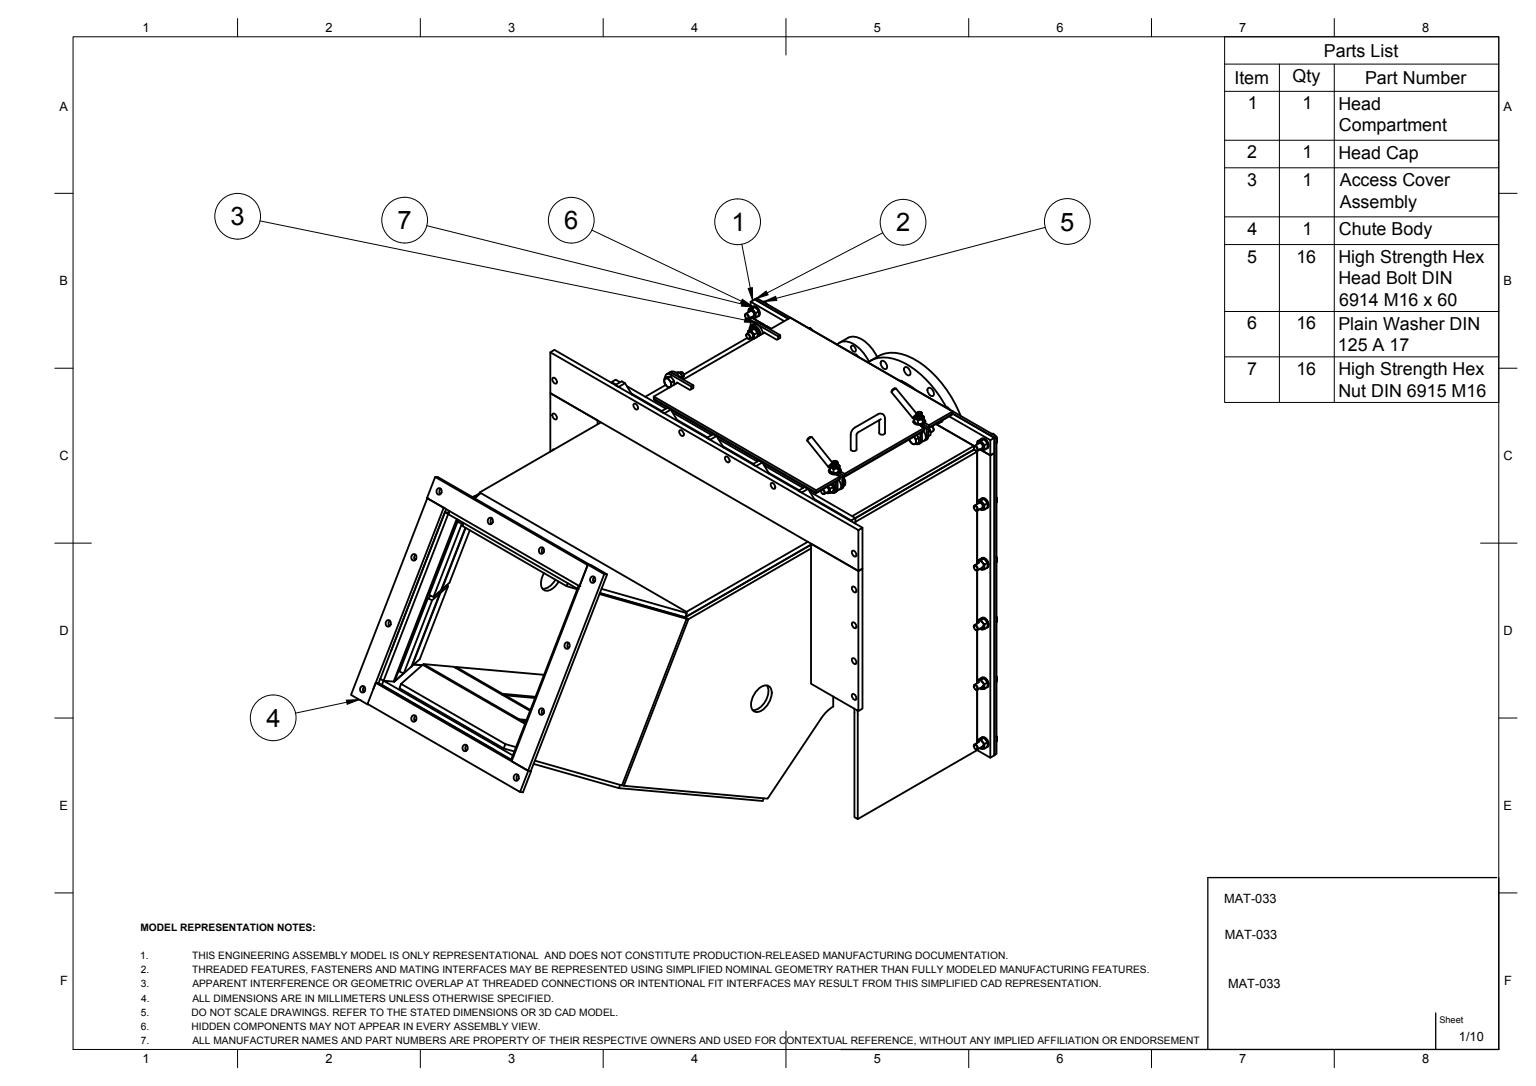
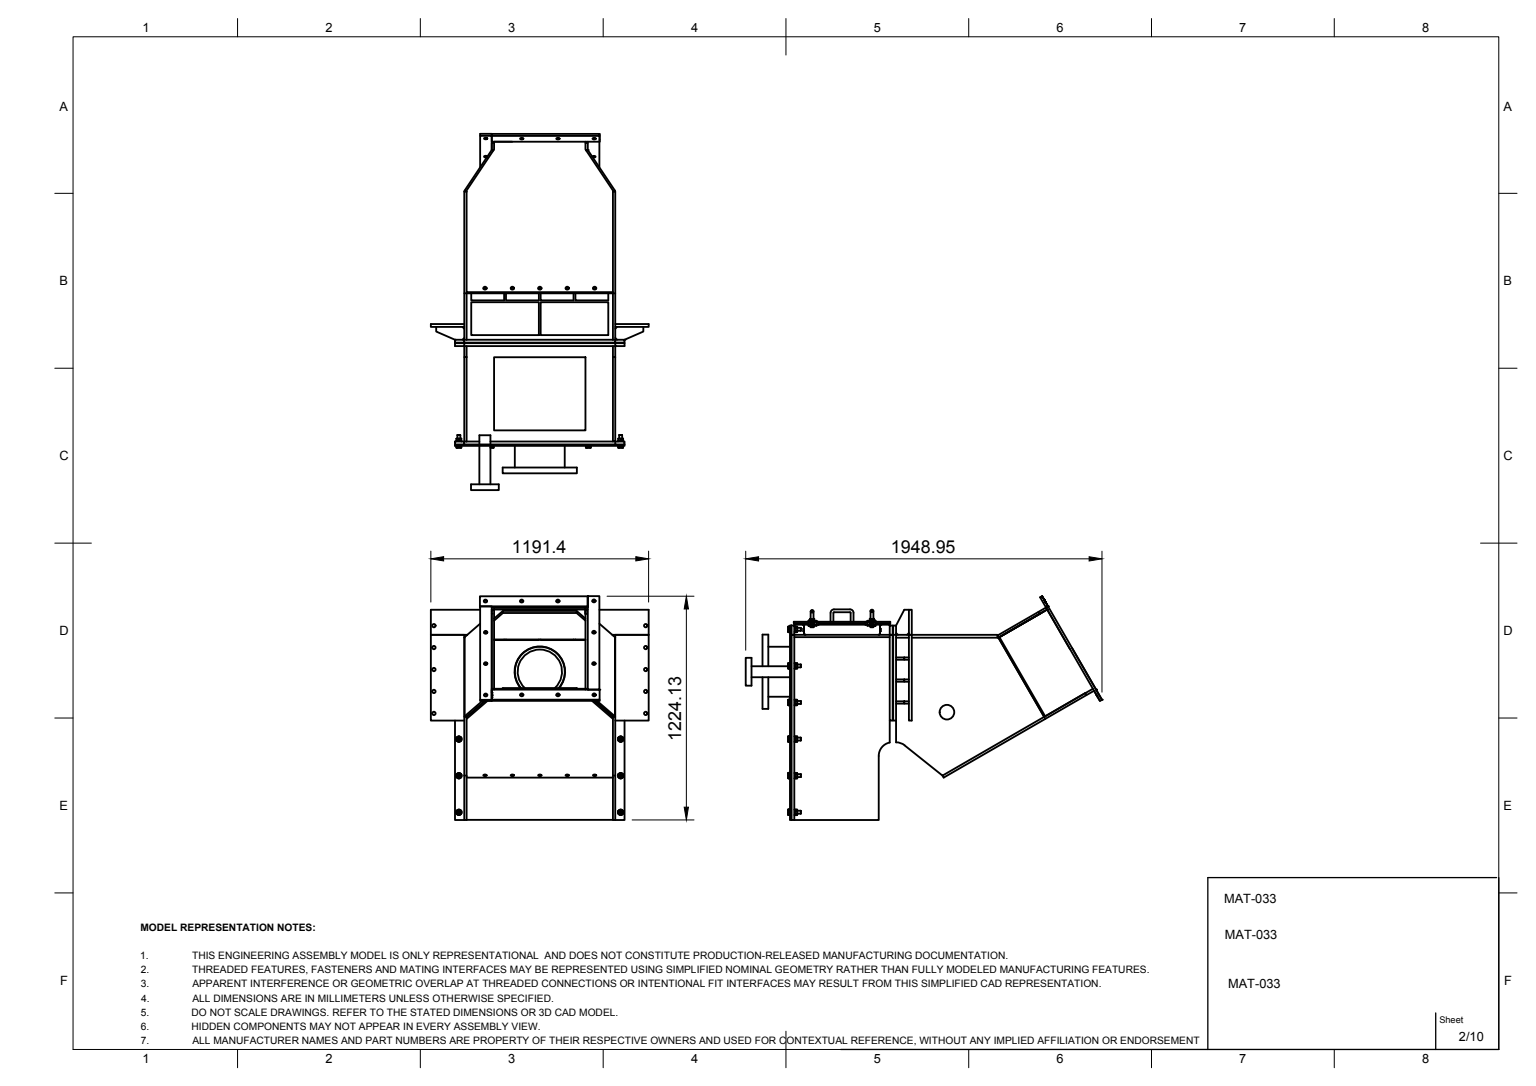
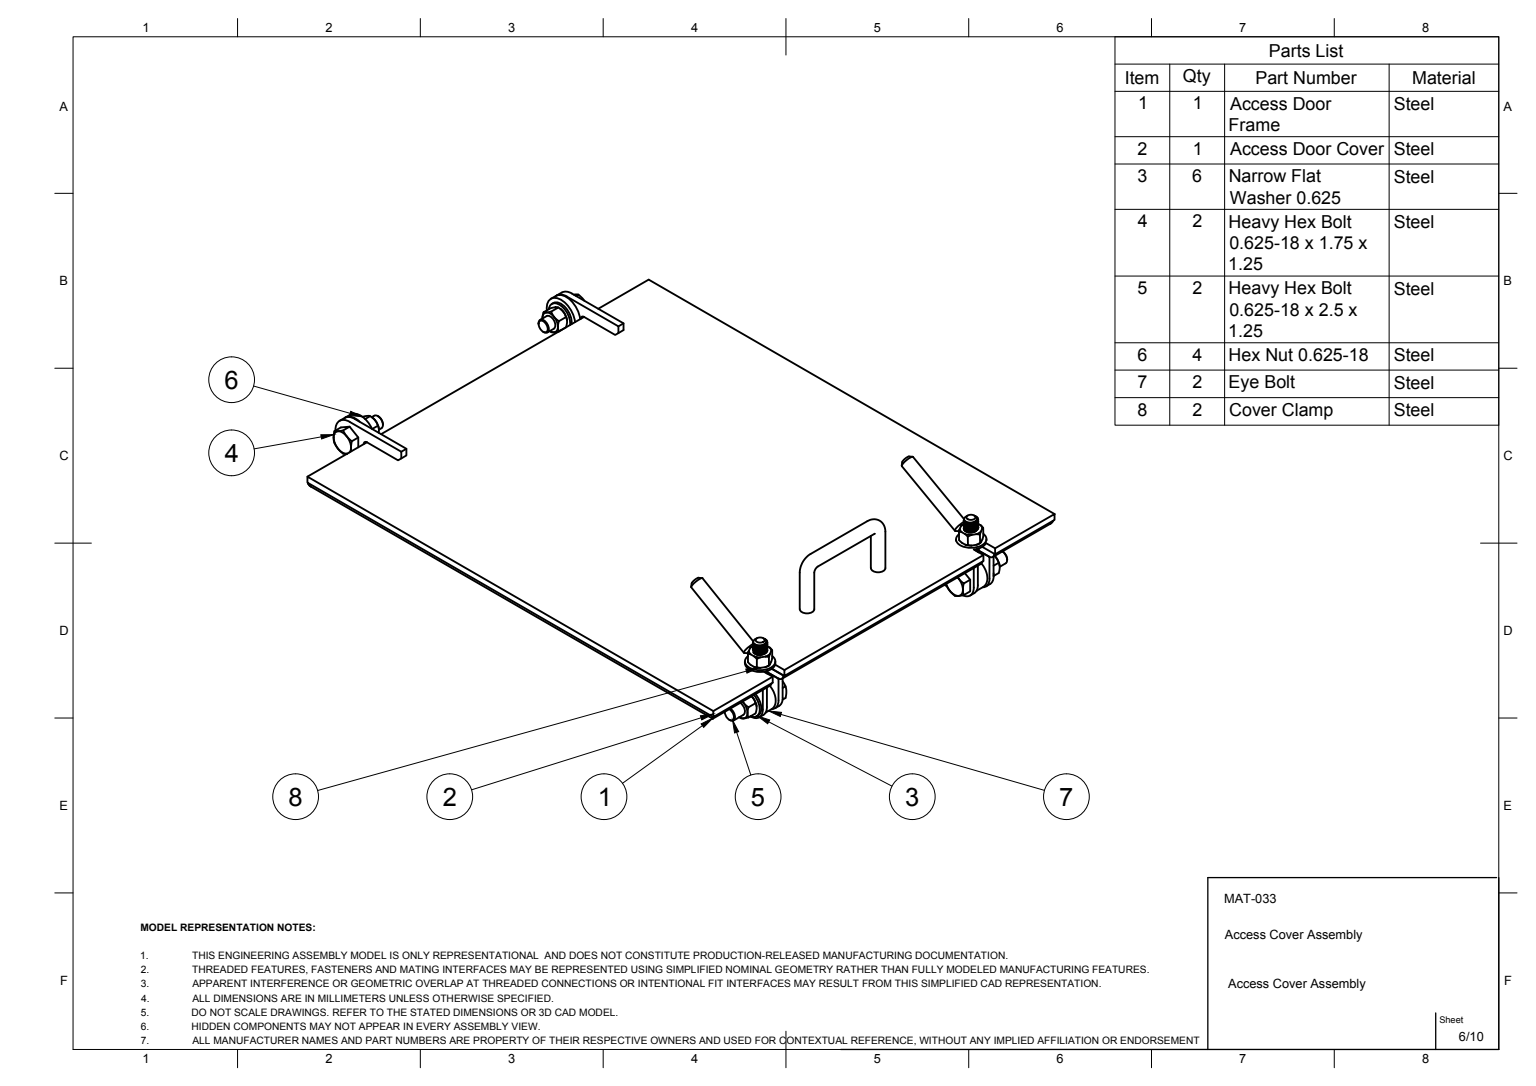
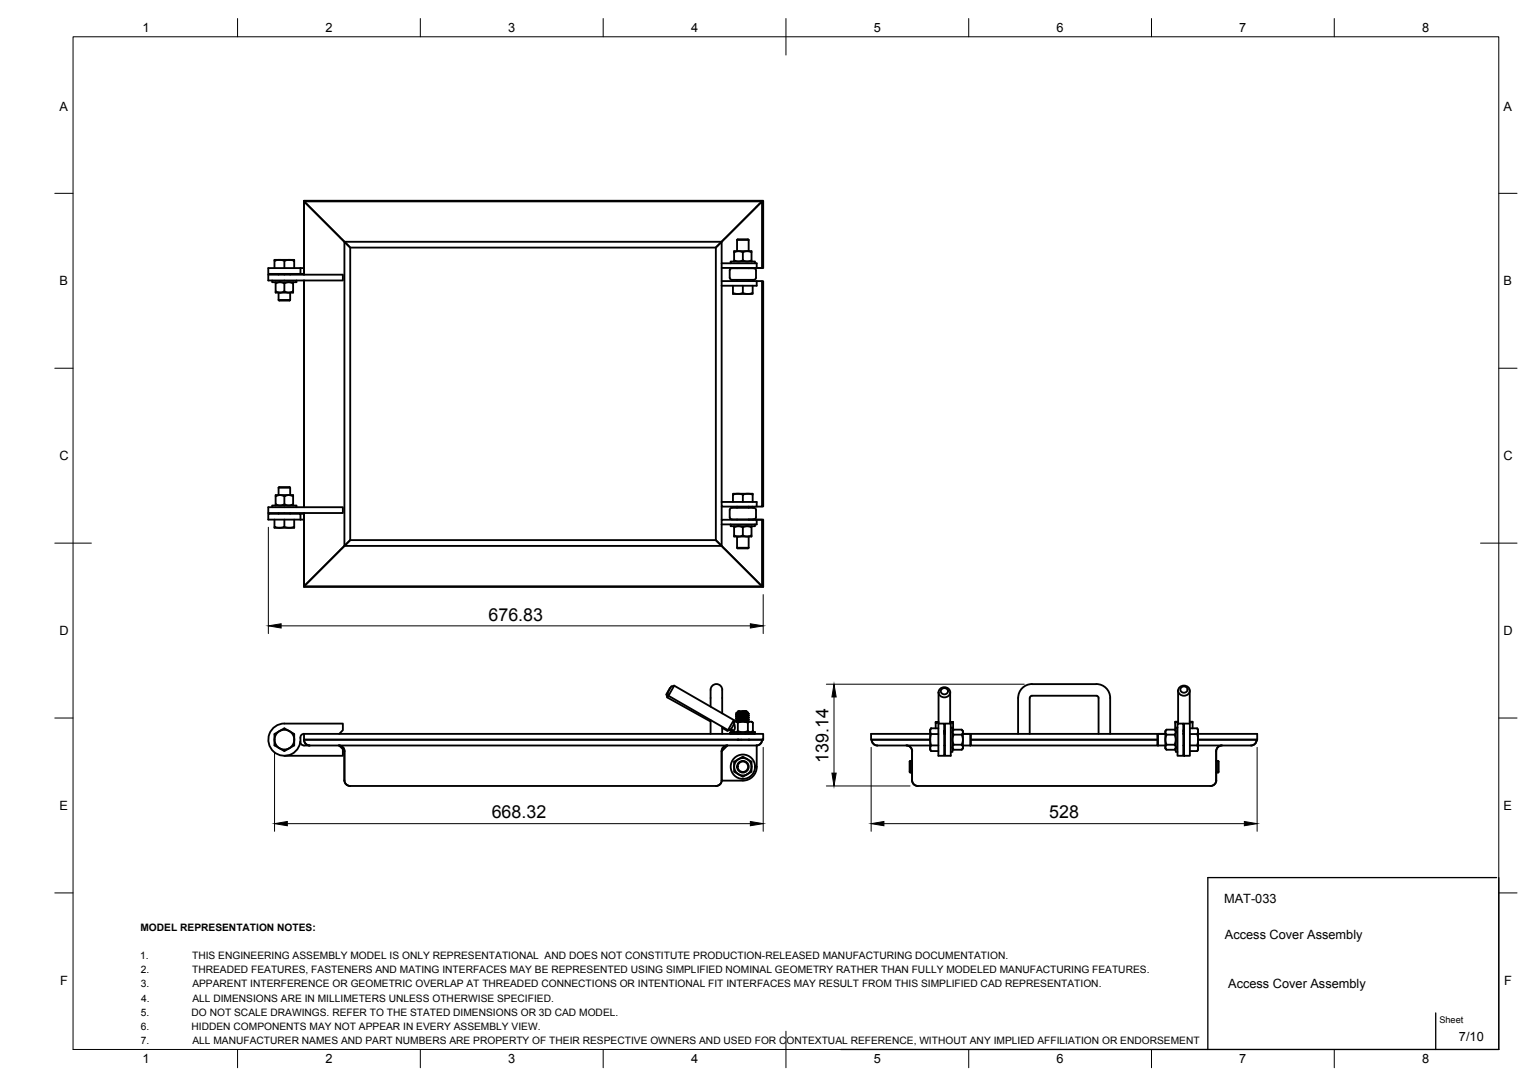
ISO-10303-21;
HEADER;
/* Generated by software containing ST-Developer
 * from STEP Tools, Inc. (www.steptools.com) 
 */

FILE_DESCRIPTION(
/* description */ ('STEP AP214'),
/* implementation_level */ '2;1');

FILE_NAME(
/* name */ 'MAT-033.step',
/* time_stamp */ '2026-11-14T07:13:32-08:00',
/* author */ (''),
/* organization */ (''),
/* preprocessor_version */ 'ST-DEVELOPER v20.2',
/* originating_system */ 'Autodesk Translation Framework v15.17.0.0',
/* authorisation */ '');

FILE_SCHEMA (('AUTOMOTIVE_DESIGN { 1 0 10303 214 3 1 1 }'));
ENDSEC;

DATA;
#10=MECHANICAL_DESIGN_GEOMETRIC_PRESENTATION_REPRESENTATION('',(#1291,#1292,
#1293,#1294,#1295,#1296,#1297,#1298,#1299,#1300,#1301,#1302,#1303,#1304,
#1305,#1306,#1307,#1308,#1309,#1310,#1311,#1312,#1313,#1314,#1315,#1316,
#1317,#1318,#1319,#1320,#1321,#1322,#1323,#1324,#1325,#1326,#1327,#1328,
#1329,#1330,#1331,#1332,#1333,#1334,#1335,#1336,#1337,#1338,#1339,#1340,
#1341,#1342,#1343,#1344,#1345,#1346,#1347,#1348,#1349,#1350,#1351,#1352,
#1353,#1354,#1355,#1356,#1357,#1358,#1359,#1360,#1361,#1362,#1363,#1364,
#1365,#1366,#1367,#1368,#1369,#1370,#1371,#1372,#1373,#1374,#1375,#1376,
#1377,#1378,#1379),#32903);
#11=ITEM_DEFINED_TRANSFORMATION($,$,#16041,#16528);
#12=ITEM_DEFINED_TRANSFORMATION($,$,#16210,#16529);
#13=ITEM_DEFINED_TRANSFORMATION($,$,#16519,#16530);
#14=ITEM_DEFINED_TRANSFORMATION($,$,#16276,#16531);
#15=ITEM_DEFINED_TRANSFORMATION($,$,#16303,#16532);
#16=ITEM_DEFINED_TRANSFORMATION($,$,#16330,#16533);
#17=ITEM_DEFINED_TRANSFORMATION($,$,#16374,#16534);
#18=ITEM_DEFINED_TRANSFORMATION($,$,#16451,#16535);
#19=ITEM_DEFINED_TRANSFORMATION($,$,#16519,#16536);
#20=ITEM_DEFINED_TRANSFORMATION($,$,#16519,#16537);
#21=ITEM_DEFINED_TRANSFORMATION($,$,#16519,#16538);
#22=ITEM_DEFINED_TRANSFORMATION($,$,#16276,#16539);
#23=ITEM_DEFINED_TRANSFORMATION($,$,#16303,#16540);
#24=ITEM_DEFINED_TRANSFORMATION($,$,#16330,#16541);
#25=ITEM_DEFINED_TRANSFORMATION($,$,#16330,#16542);
#26=ITEM_DEFINED_TRANSFORMATION($,$,#16330,#16543);
#27=ITEM_DEFINED_TRANSFORMATION($,$,#16374,#16544);
#28=ITEM_DEFINED_TRANSFORMATION($,$,#16519,#16545);
#29=ITEM_DEFINED_TRANSFORMATION($,$,#16451,#16546);
#30=ITEM_DEFINED_TRANSFORMATION($,$,#16519,#16547);
#31=ITEM_DEFINED_TRANSFORMATION($,$,#15784,#17105);
#32=ITEM_DEFINED_TRANSFORMATION($,$,#15899,#17106);
#33=ITEM_DEFINED_TRANSFORMATION($,$,#16040,#17107);
#34=ITEM_DEFINED_TRANSFORMATION($,$,#16548,#17108);
#35=ITEM_DEFINED_TRANSFORMATION($,$,#17007,#17109);
#36=ITEM_DEFINED_TRANSFORMATION($,$,#17052,#17110);
#37=ITEM_DEFINED_TRANSFORMATION($,$,#17061,#17111);
#38=ITEM_DEFINED_TRANSFORMATION($,$,#17007,#17112);
#39=ITEM_DEFINED_TRANSFORMATION($,$,#17007,#17113);
#40=ITEM_DEFINED_TRANSFORMATION($,$,#17007,#17114);
#41=ITEM_DEFINED_TRANSFORMATION($,$,#17007,#17115);
#42=ITEM_DEFINED_TRANSFORMATION($,$,#17007,#17116);
#43=ITEM_DEFINED_TRANSFORMATION($,$,#17007,#17117);
#44=ITEM_DEFINED_TRANSFORMATION($,$,#17007,#17118);
#45=ITEM_DEFINED_TRANSFORMATION($,$,#17007,#17119);
#46=ITEM_DEFINED_TRANSFORMATION($,$,#17007,#17120);
#47=ITEM_DEFINED_TRANSFORMATION($,$,#17007,#17121);
#48=ITEM_DEFINED_TRANSFORMATION($,$,#17007,#17122);
#49=ITEM_DEFINED_TRANSFORMATION($,$,#17007,#17123);
#50=ITEM_DEFINED_TRANSFORMATION($,$,#17007,#17124);
#51=ITEM_DEFINED_TRANSFORMATION($,$,#17007,#17125);
#52=ITEM_DEFINED_TRANSFORMATION($,$,#17007,#17126);
#53=ITEM_DEFINED_TRANSFORMATION($,$,#17052,#17127);
#54=ITEM_DEFINED_TRANSFORMATION($,$,#17052,#17128);
#55=ITEM_DEFINED_TRANSFORMATION($,$,#17052,#17129);
#56=ITEM_DEFINED_TRANSFORMATION($,$,#17052,#17130);
#57=ITEM_DEFINED_TRANSFORMATION($,$,#17052,#17131);
#58=ITEM_DEFINED_TRANSFORMATION($,$,#17052,#17132);
#59=ITEM_DEFINED_TRANSFORMATION($,$,#17052,#17133);
#60=ITEM_DEFINED_TRANSFORMATION($,$,#17052,#17134);
#61=ITEM_DEFINED_TRANSFORMATION($,$,#17052,#17135);
#62=ITEM_DEFINED_TRANSFORMATION($,$,#17052,#17136);
#63=ITEM_DEFINED_TRANSFORMATION($,$,#17052,#17137);
#64=ITEM_DEFINED_TRANSFORMATION($,$,#17052,#17138);
#65=ITEM_DEFINED_TRANSFORMATION($,$,#17052,#17139);
#66=ITEM_DEFINED_TRANSFORMATION($,$,#17052,#17140);
#67=ITEM_DEFINED_TRANSFORMATION($,$,#17052,#17141);
#68=ITEM_DEFINED_TRANSFORMATION($,$,#17061,#17142);
#69=ITEM_DEFINED_TRANSFORMATION($,$,#17061,#17143);
#70=ITEM_DEFINED_TRANSFORMATION($,$,#17061,#17144);
#71=ITEM_DEFINED_TRANSFORMATION($,$,#17061,#17145);
#72=ITEM_DEFINED_TRANSFORMATION($,$,#17061,#17146);
#73=ITEM_DEFINED_TRANSFORMATION($,$,#17061,#17147);
#74=ITEM_DEFINED_TRANSFORMATION($,$,#17061,#17148);
#75=ITEM_DEFINED_TRANSFORMATION($,$,#17061,#17149);
#76=ITEM_DEFINED_TRANSFORMATION($,$,#17061,#17150);
#77=ITEM_DEFINED_TRANSFORMATION($,$,#17061,#17151);
#78=ITEM_DEFINED_TRANSFORMATION($,$,#17061,#17152);
#79=ITEM_DEFINED_TRANSFORMATION($,$,#17061,#17153);
#80=ITEM_DEFINED_TRANSFORMATION($,$,#17061,#17154);
#81=ITEM_DEFINED_TRANSFORMATION($,$,#17061,#17155);
#82=ITEM_DEFINED_TRANSFORMATION($,$,#17061,#17156);
#83=(
REPRESENTATION_RELATIONSHIP($,$,#33016,#33015)
REPRESENTATION_RELATIONSHIP_WITH_TRANSFORMATION(#11)
SHAPE_REPRESENTATION_RELATIONSHIP()
);
#84=(
REPRESENTATION_RELATIONSHIP($,$,#33017,#33015)
REPRESENTATION_RELATIONSHIP_WITH_TRANSFORMATION(#12)
SHAPE_REPRESENTATION_RELATIONSHIP()
);
#85=(
REPRESENTATION_RELATIONSHIP($,$,#33023,#33015)
REPRESENTATION_RELATIONSHIP_WITH_TRANSFORMATION(#13)
SHAPE_REPRESENTATION_RELATIONSHIP()
);
#86=(
REPRESENTATION_RELATIONSHIP($,$,#33018,#33015)
REPRESENTATION_RELATIONSHIP_WITH_TRANSFORMATION(#14)
SHAPE_REPRESENTATION_RELATIONSHIP()
);
#87=(
REPRESENTATION_RELATIONSHIP($,$,#33019,#33015)
REPRESENTATION_RELATIONSHIP_WITH_TRANSFORMATION(#15)
SHAPE_REPRESENTATION_RELATIONSHIP()
);
#88=(
REPRESENTATION_RELATIONSHIP($,$,#33020,#33015)
REPRESENTATION_RELATIONSHIP_WITH_TRANSFORMATION(#16)
SHAPE_REPRESENTATION_RELATIONSHIP()
);
#89=(
REPRESENTATION_RELATIONSHIP($,$,#33021,#33015)
REPRESENTATION_RELATIONSHIP_WITH_TRANSFORMATION(#17)
SHAPE_REPRESENTATION_RELATIONSHIP()
);
#90=(
REPRESENTATION_RELATIONSHIP($,$,#33022,#33015)
REPRESENTATION_RELATIONSHIP_WITH_TRANSFORMATION(#18)
SHAPE_REPRESENTATION_RELATIONSHIP()
);
#91=(
REPRESENTATION_RELATIONSHIP($,$,#33023,#33015)
REPRESENTATION_RELATIONSHIP_WITH_TRANSFORMATION(#19)
SHAPE_REPRESENTATION_RELATIONSHIP()
);
#92=(
REPRESENTATION_RELATIONSHIP($,$,#33023,#33015)
REPRESENTATION_RELATIONSHIP_WITH_TRANSFORMATION(#20)
SHAPE_REPRESENTATION_RELATIONSHIP()
);
#93=(
REPRESENTATION_RELATIONSHIP($,$,#33023,#33015)
REPRESENTATION_RELATIONSHIP_WITH_TRANSFORMATION(#21)
SHAPE_REPRESENTATION_RELATIONSHIP()
);
#94=(
REPRESENTATION_RELATIONSHIP($,$,#33018,#33015)
REPRESENTATION_RELATIONSHIP_WITH_TRANSFORMATION(#22)
SHAPE_REPRESENTATION_RELATIONSHIP()
);
#95=(
REPRESENTATION_RELATIONSHIP($,$,#33019,#33015)
REPRESENTATION_RELATIONSHIP_WITH_TRANSFORMATION(#23)
SHAPE_REPRESENTATION_RELATIONSHIP()
);
#96=(
REPRESENTATION_RELATIONSHIP($,$,#33020,#33015)
REPRESENTATION_RELATIONSHIP_WITH_TRANSFORMATION(#24)
SHAPE_REPRESENTATION_RELATIONSHIP()
);
#97=(
REPRESENTATION_RELATIONSHIP($,$,#33020,#33015)
REPRESENTATION_RELATIONSHIP_WITH_TRANSFORMATION(#25)
SHAPE_REPRESENTATION_RELATIONSHIP()
);
#98=(
REPRESENTATION_RELATIONSHIP($,$,#33020,#33015)
REPRESENTATION_RELATIONSHIP_WITH_TRANSFORMATION(#26)
SHAPE_REPRESENTATION_RELATIONSHIP()
);
#99=(
REPRESENTATION_RELATIONSHIP($,$,#33021,#33015)
REPRESENTATION_RELATIONSHIP_WITH_TRANSFORMATION(#27)
SHAPE_REPRESENTATION_RELATIONSHIP()
);
#100=(
REPRESENTATION_RELATIONSHIP($,$,#33023,#33015)
REPRESENTATION_RELATIONSHIP_WITH_TRANSFORMATION(#28)
SHAPE_REPRESENTATION_RELATIONSHIP()
);
#101=(
REPRESENTATION_RELATIONSHIP($,$,#33022,#33015)
REPRESENTATION_RELATIONSHIP_WITH_TRANSFORMATION(#29)
SHAPE_REPRESENTATION_RELATIONSHIP()
);
#102=(
REPRESENTATION_RELATIONSHIP($,$,#33023,#33015)
REPRESENTATION_RELATIONSHIP_WITH_TRANSFORMATION(#30)
SHAPE_REPRESENTATION_RELATIONSHIP()
);
#103=(
REPRESENTATION_RELATIONSHIP($,$,#33013,#33012)
REPRESENTATION_RELATIONSHIP_WITH_TRANSFORMATION(#31)
SHAPE_REPRESENTATION_RELATIONSHIP()
);
#104=(
REPRESENTATION_RELATIONSHIP($,$,#33014,#33012)
REPRESENTATION_RELATIONSHIP_WITH_TRANSFORMATION(#32)
SHAPE_REPRESENTATION_RELATIONSHIP()
);
#105=(
REPRESENTATION_RELATIONSHIP($,$,#33015,#33012)
REPRESENTATION_RELATIONSHIP_WITH_TRANSFORMATION(#33)
SHAPE_REPRESENTATION_RELATIONSHIP()
);
#106=(
REPRESENTATION_RELATIONSHIP($,$,#33024,#33012)
REPRESENTATION_RELATIONSHIP_WITH_TRANSFORMATION(#34)
SHAPE_REPRESENTATION_RELATIONSHIP()
);
#107=(
REPRESENTATION_RELATIONSHIP($,$,#33025,#33012)
REPRESENTATION_RELATIONSHIP_WITH_TRANSFORMATION(#35)
SHAPE_REPRESENTATION_RELATIONSHIP()
);
#108=(
REPRESENTATION_RELATIONSHIP($,$,#33026,#33012)
REPRESENTATION_RELATIONSHIP_WITH_TRANSFORMATION(#36)
SHAPE_REPRESENTATION_RELATIONSHIP()
);
#109=(
REPRESENTATION_RELATIONSHIP($,$,#33027,#33012)
REPRESENTATION_RELATIONSHIP_WITH_TRANSFORMATION(#37)
SHAPE_REPRESENTATION_RELATIONSHIP()
);
#110=(
REPRESENTATION_RELATIONSHIP($,$,#33025,#33012)
REPRESENTATION_RELATIONSHIP_WITH_TRANSFORMATION(#38)
SHAPE_REPRESENTATION_RELATIONSHIP()
);
#111=(
REPRESENTATION_RELATIONSHIP($,$,#33025,#33012)
REPRESENTATION_RELATIONSHIP_WITH_TRANSFORMATION(#39)
SHAPE_REPRESENTATION_RELATIONSHIP()
);
#112=(
REPRESENTATION_RELATIONSHIP($,$,#33025,#33012)
REPRESENTATION_RELATIONSHIP_WITH_TRANSFORMATION(#40)
SHAPE_REPRESENTATION_RELATIONSHIP()
);
#113=(
REPRESENTATION_RELATIONSHIP($,$,#33025,#33012)
REPRESENTATION_RELATIONSHIP_WITH_TRANSFORMATION(#41)
SHAPE_REPRESENTATION_RELATIONSHIP()
);
#114=(
REPRESENTATION_RELATIONSHIP($,$,#33025,#33012)
REPRESENTATION_RELATIONSHIP_WITH_TRANSFORMATION(#42)
SHAPE_REPRESENTATION_RELATIONSHIP()
);
#115=(
REPRESENTATION_RELATIONSHIP($,$,#33025,#33012)
REPRESENTATION_RELATIONSHIP_WITH_TRANSFORMATION(#43)
SHAPE_REPRESENTATION_RELATIONSHIP()
);
#116=(
REPRESENTATION_RELATIONSHIP($,$,#33025,#33012)
REPRESENTATION_RELATIONSHIP_WITH_TRANSFORMATION(#44)
SHAPE_REPRESENTATION_RELATIONSHIP()
);
#117=(
REPRESENTATION_RELATIONSHIP($,$,#33025,#33012)
REPRESENTATION_RELATIONSHIP_WITH_TRANSFORMATION(#45)
SHAPE_REPRESENTATION_RELATIONSHIP()
);
#118=(
REPRESENTATION_RELATIONSHIP($,$,#33025,#33012)
REPRESENTATION_RELATIONSHIP_WITH_TRANSFORMATION(#46)
SHAPE_REPRESENTATION_RELATIONSHIP()
);
#119=(
REPRESENTATION_RELATIONSHIP($,$,#33025,#33012)
REPRESENTATION_RELATIONSHIP_WITH_TRANSFORMATION(#47)
SHAPE_REPRESENTATION_RELATIONSHIP()
);
#120=(
REPRESENTATION_RELATIONSHIP($,$,#33025,#33012)
REPRESENTATION_RELATIONSHIP_WITH_TRANSFORMATION(#48)
SHAPE_REPRESENTATION_RELATIONSHIP()
);
#121=(
REPRESENTATION_RELATIONSHIP($,$,#33025,#33012)
REPRESENTATION_RELATIONSHIP_WITH_TRANSFORMATION(#49)
SHAPE_REPRESENTATION_RELATIONSHIP()
);
#122=(
REPRESENTATION_RELATIONSHIP($,$,#33025,#33012)
REPRESENTATION_RELATIONSHIP_WITH_TRANSFORMATION(#50)
SHAPE_REPRESENTATION_RELATIONSHIP()
);
#123=(
REPRESENTATION_RELATIONSHIP($,$,#33025,#33012)
REPRESENTATION_RELATIONSHIP_WITH_TRANSFORMATION(#51)
SHAPE_REPRESENTATION_RELATIONSHIP()
);
#124=(
REPRESENTATION_RELATIONSHIP($,$,#33025,#33012)
REPRESENTATION_RELATIONSHIP_WITH_TRANSFORMATION(#52)
SHAPE_REPRESENTATION_RELATIONSHIP()
);
#125=(
REPRESENTATION_RELATIONSHIP($,$,#33026,#33012)
REPRESENTATION_RELATIONSHIP_WITH_TRANSFORMATION(#53)
SHAPE_REPRESENTATION_RELATIONSHIP()
);
#126=(
REPRESENTATION_RELATIONSHIP($,$,#33026,#33012)
REPRESENTATION_RELATIONSHIP_WITH_TRANSFORMATION(#54)
SHAPE_REPRESENTATION_RELATIONSHIP()
);
#127=(
REPRESENTATION_RELATIONSHIP($,$,#33026,#33012)
REPRESENTATION_RELATIONSHIP_WITH_TRANSFORMATION(#55)
SHAPE_REPRESENTATION_RELATIONSHIP()
);
#128=(
REPRESENTATION_RELATIONSHIP($,$,#33026,#33012)
REPRESENTATION_RELATIONSHIP_WITH_TRANSFORMATION(#56)
SHAPE_REPRESENTATION_RELATIONSHIP()
);
#129=(
REPRESENTATION_RELATIONSHIP($,$,#33026,#33012)
REPRESENTATION_RELATIONSHIP_WITH_TRANSFORMATION(#57)
SHAPE_REPRESENTATION_RELATIONSHIP()
);
#130=(
REPRESENTATION_RELATIONSHIP($,$,#33026,#33012)
REPRESENTATION_RELATIONSHIP_WITH_TRANSFORMATION(#58)
SHAPE_REPRESENTATION_RELATIONSHIP()
);
#131=(
REPRESENTATION_RELATIONSHIP($,$,#33026,#33012)
REPRESENTATION_RELATIONSHIP_WITH_TRANSFORMATION(#59)
SHAPE_REPRESENTATION_RELATIONSHIP()
);
#132=(
REPRESENTATION_RELATIONSHIP($,$,#33026,#33012)
REPRESENTATION_RELATIONSHIP_WITH_TRANSFORMATION(#60)
SHAPE_REPRESENTATION_RELATIONSHIP()
);
#133=(
REPRESENTATION_RELATIONSHIP($,$,#33026,#33012)
REPRESENTATION_RELATIONSHIP_WITH_TRANSFORMATION(#61)
SHAPE_REPRESENTATION_RELATIONSHIP()
);
#134=(
REPRESENTATION_RELATIONSHIP($,$,#33026,#33012)
REPRESENTATION_RELATIONSHIP_WITH_TRANSFORMATION(#62)
SHAPE_REPRESENTATION_RELATIONSHIP()
);
#135=(
REPRESENTATION_RELATIONSHIP($,$,#33026,#33012)
REPRESENTATION_RELATIONSHIP_WITH_TRANSFORMATION(#63)
SHAPE_REPRESENTATION_RELATIONSHIP()
);
#136=(
REPRESENTATION_RELATIONSHIP($,$,#33026,#33012)
REPRESENTATION_RELATIONSHIP_WITH_TRANSFORMATION(#64)
SHAPE_REPRESENTATION_RELATIONSHIP()
);
#137=(
REPRESENTATION_RELATIONSHIP($,$,#33026,#33012)
REPRESENTATION_RELATIONSHIP_WITH_TRANSFORMATION(#65)
SHAPE_REPRESENTATION_RELATIONSHIP()
);
#138=(
REPRESENTATION_RELATIONSHIP($,$,#33026,#33012)
REPRESENTATION_RELATIONSHIP_WITH_TRANSFORMATION(#66)
SHAPE_REPRESENTATION_RELATIONSHIP()
);
#139=(
REPRESENTATION_RELATIONSHIP($,$,#33026,#33012)
REPRESENTATION_RELATIONSHIP_WITH_TRANSFORMATION(#67)
SHAPE_REPRESENTATION_RELATIONSHIP()
);
#140=(
REPRESENTATION_RELATIONSHIP($,$,#33027,#33012)
REPRESENTATION_RELATIONSHIP_WITH_TRANSFORMATION(#68)
SHAPE_REPRESENTATION_RELATIONSHIP()
);
#141=(
REPRESENTATION_RELATIONSHIP($,$,#33027,#33012)
REPRESENTATION_RELATIONSHIP_WITH_TRANSFORMATION(#69)
SHAPE_REPRESENTATION_RELATIONSHIP()
);
#142=(
REPRESENTATION_RELATIONSHIP($,$,#33027,#33012)
REPRESENTATION_RELATIONSHIP_WITH_TRANSFORMATION(#70)
SHAPE_REPRESENTATION_RELATIONSHIP()
);
#143=(
REPRESENTATION_RELATIONSHIP($,$,#33027,#33012)
REPRESENTATION_RELATIONSHIP_WITH_TRANSFORMATION(#71)
SHAPE_REPRESENTATION_RELATIONSHIP()
);
#144=(
REPRESENTATION_RELATIONSHIP($,$,#33027,#33012)
REPRESENTATION_RELATIONSHIP_WITH_TRANSFORMATION(#72)
SHAPE_REPRESENTATION_RELATIONSHIP()
);
#145=(
REPRESENTATION_RELATIONSHIP($,$,#33027,#33012)
REPRESENTATION_RELATIONSHIP_WITH_TRANSFORMATION(#73)
SHAPE_REPRESENTATION_RELATIONSHIP()
);
#146=(
REPRESENTATION_RELATIONSHIP($,$,#33027,#33012)
REPRESENTATION_RELATIONSHIP_WITH_TRANSFORMATION(#74)
SHAPE_REPRESENTATION_RELATIONSHIP()
);
#147=(
REPRESENTATION_RELATIONSHIP($,$,#33027,#33012)
REPRESENTATION_RELATIONSHIP_WITH_TRANSFORMATION(#75)
SHAPE_REPRESENTATION_RELATIONSHIP()
);
#148=(
REPRESENTATION_RELATIONSHIP($,$,#33027,#33012)
REPRESENTATION_RELATIONSHIP_WITH_TRANSFORMATION(#76)
SHAPE_REPRESENTATION_RELATIONSHIP()
);
#149=(
REPRESENTATION_RELATIONSHIP($,$,#33027,#33012)
REPRESENTATION_RELATIONSHIP_WITH_TRANSFORMATION(#77)
SHAPE_REPRESENTATION_RELATIONSHIP()
);
#150=(
REPRESENTATION_RELATIONSHIP($,$,#33027,#33012)
REPRESENTATION_RELATIONSHIP_WITH_TRANSFORMATION(#78)
SHAPE_REPRESENTATION_RELATIONSHIP()
);
#151=(
REPRESENTATION_RELATIONSHIP($,$,#33027,#33012)
REPRESENTATION_RELATIONSHIP_WITH_TRANSFORMATION(#79)
SHAPE_REPRESENTATION_RELATIONSHIP()
);
#152=(
REPRESENTATION_RELATIONSHIP($,$,#33027,#33012)
REPRESENTATION_RELATIONSHIP_WITH_TRANSFORMATION(#80)
SHAPE_REPRESENTATION_RELATIONSHIP()
);
#153=(
REPRESENTATION_RELATIONSHIP($,$,#33027,#33012)
REPRESENTATION_RELATIONSHIP_WITH_TRANSFORMATION(#81)
SHAPE_REPRESENTATION_RELATIONSHIP()
);
#154=(
REPRESENTATION_RELATIONSHIP($,$,#33027,#33012)
REPRESENTATION_RELATIONSHIP_WITH_TRANSFORMATION(#82)
SHAPE_REPRESENTATION_RELATIONSHIP()
);
#155=CONTEXT_DEPENDENT_SHAPE_REPRESENTATION(#83,#32936);
#156=CONTEXT_DEPENDENT_SHAPE_REPRESENTATION(#84,#32937);
#157=CONTEXT_DEPENDENT_SHAPE_REPRESENTATION(#85,#32938);
#158=CONTEXT_DEPENDENT_SHAPE_REPRESENTATION(#86,#32939);
#159=CONTEXT_DEPENDENT_SHAPE_REPRESENTATION(#87,#32940);
#160=CONTEXT_DEPENDENT_SHAPE_REPRESENTATION(#88,#32941);
#161=CONTEXT_DEPENDENT_SHAPE_REPRESENTATION(#89,#32942);
#162=CONTEXT_DEPENDENT_SHAPE_REPRESENTATION(#90,#32943);
#163=CONTEXT_DEPENDENT_SHAPE_REPRESENTATION(#91,#32944);
#164=CONTEXT_DEPENDENT_SHAPE_REPRESENTATION(#92,#32945);
#165=CONTEXT_DEPENDENT_SHAPE_REPRESENTATION(#93,#32946);
#166=CONTEXT_DEPENDENT_SHAPE_REPRESENTATION(#94,#32947);
#167=CONTEXT_DEPENDENT_SHAPE_REPRESENTATION(#95,#32948);
#168=CONTEXT_DEPENDENT_SHAPE_REPRESENTATION(#96,#32949);
#169=CONTEXT_DEPENDENT_SHAPE_REPRESENTATION(#97,#32950);
#170=CONTEXT_DEPENDENT_SHAPE_REPRESENTATION(#98,#32951);
#171=CONTEXT_DEPENDENT_SHAPE_REPRESENTATION(#99,#32952);
#172=CONTEXT_DEPENDENT_SHAPE_REPRESENTATION(#100,#32953);
#173=CONTEXT_DEPENDENT_SHAPE_REPRESENTATION(#101,#32954);
#174=CONTEXT_DEPENDENT_SHAPE_REPRESENTATION(#102,#32955);
#175=CONTEXT_DEPENDENT_SHAPE_REPRESENTATION(#103,#32960);
#176=CONTEXT_DEPENDENT_SHAPE_REPRESENTATION(#104,#32961);
#177=CONTEXT_DEPENDENT_SHAPE_REPRESENTATION(#105,#32962);
#178=CONTEXT_DEPENDENT_SHAPE_REPRESENTATION(#106,#32963);
#179=CONTEXT_DEPENDENT_SHAPE_REPRESENTATION(#107,#32964);
#180=CONTEXT_DEPENDENT_SHAPE_REPRESENTATION(#108,#32965);
#181=CONTEXT_DEPENDENT_SHAPE_REPRESENTATION(#109,#32966);
#182=CONTEXT_DEPENDENT_SHAPE_REPRESENTATION(#110,#32967);
#183=CONTEXT_DEPENDENT_SHAPE_REPRESENTATION(#111,#32968);
#184=CONTEXT_DEPENDENT_SHAPE_REPRESENTATION(#112,#32969);
#185=CONTEXT_DEPENDENT_SHAPE_REPRESENTATION(#113,#32970);
#186=CONTEXT_DEPENDENT_SHAPE_REPRESENTATION(#114,#32971);
#187=CONTEXT_DEPENDENT_SHAPE_REPRESENTATION(#115,#32972);
#188=CONTEXT_DEPENDENT_SHAPE_REPRESENTATION(#116,#32973);
#189=CONTEXT_DEPENDENT_SHAPE_REPRESENTATION(#117,#32974);
#190=CONTEXT_DEPENDENT_SHAPE_REPRESENTATION(#118,#32975);
#191=CONTEXT_DEPENDENT_SHAPE_REPRESENTATION(#119,#32976);
#192=CONTEXT_DEPENDENT_SHAPE_REPRESENTATION(#120,#32977);
#193=CONTEXT_DEPENDENT_SHAPE_REPRESENTATION(#121,#32978);
#194=CONTEXT_DEPENDENT_SHAPE_REPRESENTATION(#122,#32979);
#195=CONTEXT_DEPENDENT_SHAPE_REPRESENTATION(#123,#32980);
#196=CONTEXT_DEPENDENT_SHAPE_REPRESENTATION(#124,#32981);
#197=CONTEXT_DEPENDENT_SHAPE_REPRESENTATION(#125,#32982);
#198=CONTEXT_DEPENDENT_SHAPE_REPRESENTATION(#126,#32983);
#199=CONTEXT_DEPENDENT_SHAPE_REPRESENTATION(#127,#32984);
#200=CONTEXT_DEPENDENT_SHAPE_REPRESENTATION(#128,#32985);
#201=CONTEXT_DEPENDENT_SHAPE_REPRESENTATION(#129,#32986);
#202=CONTEXT_DEPENDENT_SHAPE_REPRESENTATION(#130,#32987);
#203=CONTEXT_DEPENDENT_SHAPE_REPRESENTATION(#131,#32988);
#204=CONTEXT_DEPENDENT_SHAPE_REPRESENTATION(#132,#32989);
#205=CONTEXT_DEPENDENT_SHAPE_REPRESENTATION(#133,#32990);
#206=CONTEXT_DEPENDENT_SHAPE_REPRESENTATION(#134,#32991);
#207=CONTEXT_DEPENDENT_SHAPE_REPRESENTATION(#135,#32992);
#208=CONTEXT_DEPENDENT_SHAPE_REPRESENTATION(#136,#32993);
#209=CONTEXT_DEPENDENT_SHAPE_REPRESENTATION(#137,#32994);
#210=CONTEXT_DEPENDENT_SHAPE_REPRESENTATION(#138,#32995);
#211=CONTEXT_DEPENDENT_SHAPE_REPRESENTATION(#139,#32996);
#212=CONTEXT_DEPENDENT_SHAPE_REPRESENTATION(#140,#32997);
#213=CONTEXT_DEPENDENT_SHAPE_REPRESENTATION(#141,#32998);
#214=CONTEXT_DEPENDENT_SHAPE_REPRESENTATION(#142,#32999);
#215=CONTEXT_DEPENDENT_SHAPE_REPRESENTATION(#143,#33000);
#216=CONTEXT_DEPENDENT_SHAPE_REPRESENTATION(#144,#33001);
#217=CONTEXT_DEPENDENT_SHAPE_REPRESENTATION(#145,#33002);
#218=CONTEXT_DEPENDENT_SHAPE_REPRESENTATION(#146,#33003);
#219=CONTEXT_DEPENDENT_SHAPE_REPRESENTATION(#147,#33004);
#220=CONTEXT_DEPENDENT_SHAPE_REPRESENTATION(#148,#33005);
#221=CONTEXT_DEPENDENT_SHAPE_REPRESENTATION(#149,#33006);
#222=CONTEXT_DEPENDENT_SHAPE_REPRESENTATION(#150,#33007);
#223=CONTEXT_DEPENDENT_SHAPE_REPRESENTATION(#151,#33008);
#224=CONTEXT_DEPENDENT_SHAPE_REPRESENTATION(#152,#33009);
#225=CONTEXT_DEPENDENT_SHAPE_REPRESENTATION(#153,#33010);
#226=CONTEXT_DEPENDENT_SHAPE_REPRESENTATION(#154,#33011);
#227=NEXT_ASSEMBLY_USAGE_OCCURRENCE('Access Door Frame:1',
'Access Door Frame:1','Access Door Frame:1',#33032,#33033,
'Access Door Frame:1');
#228=NEXT_ASSEMBLY_USAGE_OCCURRENCE('Access Door Cover:1',
'Access Door Cover:1','Access Door Cover:1',#33032,#33034,
'Access Door Cover:1');
#229=NEXT_ASSEMBLY_USAGE_OCCURRENCE('Narrow Flat Washer 0.625:1',
'Narrow Flat Washer 0.625:1','Narrow Flat Washer 0.625:1',#33032,#33040,
'Narrow Flat Washer 0.625:1');
#230=NEXT_ASSEMBLY_USAGE_OCCURRENCE(
'Heavy Hex Bolt 0.625-18 x 1.75 x 1.25:1',
'Heavy Hex Bolt 0.625-18 x 1.75 x 1.25:1',
'Heavy Hex Bolt 0.625-18 x 1.75 x 1.25:1',#33032,#33035,
'Heavy Hex Bolt 0.625-18 x 1.75 x 1.25:1');
#231=NEXT_ASSEMBLY_USAGE_OCCURRENCE(
'Heavy Hex Bolt 0.625-18 x 2.5 x 1.25:1',
'Heavy Hex Bolt 0.625-18 x 2.5 x 1.25:1',
'Heavy Hex Bolt 0.625-18 x 2.5 x 1.25:1',#33032,#33036,
'Heavy Hex Bolt 0.625-18 x 2.5 x 1.25:1');
#232=NEXT_ASSEMBLY_USAGE_OCCURRENCE('Hex Nut 0.625-18:1',
'Hex Nut 0.625-18:1','Hex Nut 0.625-18:1',#33032,#33037,
'Hex Nut 0.625-18:1');
#233=NEXT_ASSEMBLY_USAGE_OCCURRENCE('Eye Bolt:1','Eye Bolt:1',
'Eye Bolt:1',#33032,#33038,'Eye Bolt:1');
#234=NEXT_ASSEMBLY_USAGE_OCCURRENCE('Cover Clamp:1','Cover Clamp:1',
'Cover Clamp:1',#33032,#33039,'Cover Clamp:1');
#235=NEXT_ASSEMBLY_USAGE_OCCURRENCE('Narrow Flat Washer 0.625:2',
'Narrow Flat Washer 0.625:2','Narrow Flat Washer 0.625:2',#33032,#33040,
'Narrow Flat Washer 0.625:2');
#236=NEXT_ASSEMBLY_USAGE_OCCURRENCE('Narrow Flat Washer 0.625:3',
'Narrow Flat Washer 0.625:3','Narrow Flat Washer 0.625:3',#33032,#33040,
'Narrow Flat Washer 0.625:3');
#237=NEXT_ASSEMBLY_USAGE_OCCURRENCE('Narrow Flat Washer 0.625:4',
'Narrow Flat Washer 0.625:4','Narrow Flat Washer 0.625:4',#33032,#33040,
'Narrow Flat Washer 0.625:4');
#238=NEXT_ASSEMBLY_USAGE_OCCURRENCE(
'Heavy Hex Bolt 0.625-18 x 1.75 x 1.25:2',
'Heavy Hex Bolt 0.625-18 x 1.75 x 1.25:2',
'Heavy Hex Bolt 0.625-18 x 1.75 x 1.25:2',#33032,#33035,
'Heavy Hex Bolt 0.625-18 x 1.75 x 1.25:2');
#239=NEXT_ASSEMBLY_USAGE_OCCURRENCE(
'Heavy Hex Bolt 0.625-18 x 2.5 x 1.25:2',
'Heavy Hex Bolt 0.625-18 x 2.5 x 1.25:2',
'Heavy Hex Bolt 0.625-18 x 2.5 x 1.25:2',#33032,#33036,
'Heavy Hex Bolt 0.625-18 x 2.5 x 1.25:2');
#240=NEXT_ASSEMBLY_USAGE_OCCURRENCE('Hex Nut 0.625-18:2',
'Hex Nut 0.625-18:2','Hex Nut 0.625-18:2',#33032,#33037,
'Hex Nut 0.625-18:2');
#241=NEXT_ASSEMBLY_USAGE_OCCURRENCE('Hex Nut 0.625-18:3',
'Hex Nut 0.625-18:3','Hex Nut 0.625-18:3',#33032,#33037,
'Hex Nut 0.625-18:3');
#242=NEXT_ASSEMBLY_USAGE_OCCURRENCE('Hex Nut 0.625-18:4',
'Hex Nut 0.625-18:4','Hex Nut 0.625-18:4',#33032,#33037,
'Hex Nut 0.625-18:4');
#243=NEXT_ASSEMBLY_USAGE_OCCURRENCE('Eye Bolt:2','Eye Bolt:2',
'Eye Bolt:2',#33032,#33038,'Eye Bolt:2');
#244=NEXT_ASSEMBLY_USAGE_OCCURRENCE('Narrow Flat Washer 0.625:5',
'Narrow Flat Washer 0.625:5','Narrow Flat Washer 0.625:5',#33032,#33040,
'Narrow Flat Washer 0.625:5');
#245=NEXT_ASSEMBLY_USAGE_OCCURRENCE('Cover Clamp:2','Cover Clamp:2',
'Cover Clamp:2',#33032,#33039,'Cover Clamp:2');
#246=NEXT_ASSEMBLY_USAGE_OCCURRENCE('Narrow Flat Washer 0.625:6',
'Narrow Flat Washer 0.625:6','Narrow Flat Washer 0.625:6',#33032,#33040,
'Narrow Flat Washer 0.625:6');
#247=NEXT_ASSEMBLY_USAGE_OCCURRENCE('Head Compartment:1',
'Head Compartment:1','Head Compartment:1',#33029,#33030,
'Head Compartment:1');
#248=NEXT_ASSEMBLY_USAGE_OCCURRENCE('Head Cap:1','Head Cap:1',
'Head Cap:1',#33029,#33031,'Head Cap:1');
#249=NEXT_ASSEMBLY_USAGE_OCCURRENCE('Access Cover Assembly:1',
'Access Cover Assembly:1','Access Cover Assembly:1',#33029,#33032,
'Access Cover Assembly:1');
#250=NEXT_ASSEMBLY_USAGE_OCCURRENCE('Chute Body:1','Chute Body:1',
'Chute Body:1',#33029,#33041,'Chute Body:1');
#251=NEXT_ASSEMBLY_USAGE_OCCURRENCE(
'High Strength Hex Head Bolt DIN 6914 M16 x 60:1',
'High Strength Hex Head Bolt DIN 6914 M16 x 60:1',
'High Strength Hex Head Bolt DIN 6914 M16 x 60:1',#33029,#33042,
'High Strength Hex Head Bolt DIN 6914 M16 x 60:1');
#252=NEXT_ASSEMBLY_USAGE_OCCURRENCE('Plain Washer DIN 125 A 17:1',
'Plain Washer DIN 125 A 17:1','Plain Washer DIN 125 A 17:1',#33029,#33043,
'Plain Washer DIN 125 A 17:1');
#253=NEXT_ASSEMBLY_USAGE_OCCURRENCE(
'High Strength Hex Nut DIN 6915 M16:1',
'High Strength Hex Nut DIN 6915 M16:1',
'High Strength Hex Nut DIN 6915 M16:1',#33029,#33044,
'High Strength Hex Nut DIN 6915 M16:1');
#254=NEXT_ASSEMBLY_USAGE_OCCURRENCE(
'High Strength Hex Head Bolt DIN 6914 M16 x 60:2',
'High Strength Hex Head Bolt DIN 6914 M16 x 60:2',
'High Strength Hex Head Bolt DIN 6914 M16 x 60:2',#33029,#33042,
'High Strength Hex Head Bolt DIN 6914 M16 x 60:2');
#255=NEXT_ASSEMBLY_USAGE_OCCURRENCE(
'High Strength Hex Head Bolt DIN 6914 M16 x 60:3',
'High Strength Hex Head Bolt DIN 6914 M16 x 60:3',
'High Strength Hex Head Bolt DIN 6914 M16 x 60:3',#33029,#33042,
'High Strength Hex Head Bolt DIN 6914 M16 x 60:3');
#256=NEXT_ASSEMBLY_USAGE_OCCURRENCE(
'High Strength Hex Head Bolt DIN 6914 M16 x 60:4',
'High Strength Hex Head Bolt DIN 6914 M16 x 60:4',
'High Strength Hex Head Bolt DIN 6914 M16 x 60:4',#33029,#33042,
'High Strength Hex Head Bolt DIN 6914 M16 x 60:4');
#257=NEXT_ASSEMBLY_USAGE_OCCURRENCE(
'High Strength Hex Head Bolt DIN 6914 M16 x 60:5',
'High Strength Hex Head Bolt DIN 6914 M16 x 60:5',
'High Strength Hex Head Bolt DIN 6914 M16 x 60:5',#33029,#33042,
'High Strength Hex Head Bolt DIN 6914 M16 x 60:5');
#258=NEXT_ASSEMBLY_USAGE_OCCURRENCE(
'High Strength Hex Head Bolt DIN 6914 M16 x 60:6',
'High Strength Hex Head Bolt DIN 6914 M16 x 60:6',
'High Strength Hex Head Bolt DIN 6914 M16 x 60:6',#33029,#33042,
'High Strength Hex Head Bolt DIN 6914 M16 x 60:6');
#259=NEXT_ASSEMBLY_USAGE_OCCURRENCE(
'High Strength Hex Head Bolt DIN 6914 M16 x 60:7',
'High Strength Hex Head Bolt DIN 6914 M16 x 60:7',
'High Strength Hex Head Bolt DIN 6914 M16 x 60:7',#33029,#33042,
'High Strength Hex Head Bolt DIN 6914 M16 x 60:7');
#260=NEXT_ASSEMBLY_USAGE_OCCURRENCE(
'High Strength Hex Head Bolt DIN 6914 M16 x 60:8',
'High Strength Hex Head Bolt DIN 6914 M16 x 60:8',
'High Strength Hex Head Bolt DIN 6914 M16 x 60:8',#33029,#33042,
'High Strength Hex Head Bolt DIN 6914 M16 x 60:8');
#261=NEXT_ASSEMBLY_USAGE_OCCURRENCE(
'High Strength Hex Head Bolt DIN 6914 M16 x 60:9',
'High Strength Hex Head Bolt DIN 6914 M16 x 60:9',
'High Strength Hex Head Bolt DIN 6914 M16 x 60:9',#33029,#33042,
'High Strength Hex Head Bolt DIN 6914 M16 x 60:9');
#262=NEXT_ASSEMBLY_USAGE_OCCURRENCE(
'High Strength Hex Head Bolt DIN 6914 M16 x 60:10',
'High Strength Hex Head Bolt DIN 6914 M16 x 60:10',
'High Strength Hex Head Bolt DIN 6914 M16 x 60:10',#33029,#33042,
'High Strength Hex Head Bolt DIN 6914 M16 x 60:10');
#263=NEXT_ASSEMBLY_USAGE_OCCURRENCE(
'High Strength Hex Head Bolt DIN 6914 M16 x 60:11',
'High Strength Hex Head Bolt DIN 6914 M16 x 60:11',
'High Strength Hex Head Bolt DIN 6914 M16 x 60:11',#33029,#33042,
'High Strength Hex Head Bolt DIN 6914 M16 x 60:11');
#264=NEXT_ASSEMBLY_USAGE_OCCURRENCE(
'High Strength Hex Head Bolt DIN 6914 M16 x 60:12',
'High Strength Hex Head Bolt DIN 6914 M16 x 60:12',
'High Strength Hex Head Bolt DIN 6914 M16 x 60:12',#33029,#33042,
'High Strength Hex Head Bolt DIN 6914 M16 x 60:12');
#265=NEXT_ASSEMBLY_USAGE_OCCURRENCE(
'High Strength Hex Head Bolt DIN 6914 M16 x 60:13',
'High Strength Hex Head Bolt DIN 6914 M16 x 60:13',
'High Strength Hex Head Bolt DIN 6914 M16 x 60:13',#33029,#33042,
'High Strength Hex Head Bolt DIN 6914 M16 x 60:13');
#266=NEXT_ASSEMBLY_USAGE_OCCURRENCE(
'High Strength Hex Head Bolt DIN 6914 M16 x 60:14',
'High Strength Hex Head Bolt DIN 6914 M16 x 60:14',
'High Strength Hex Head Bolt DIN 6914 M16 x 60:14',#33029,#33042,
'High Strength Hex Head Bolt DIN 6914 M16 x 60:14');
#267=NEXT_ASSEMBLY_USAGE_OCCURRENCE(
'High Strength Hex Head Bolt DIN 6914 M16 x 60:15',
'High Strength Hex Head Bolt DIN 6914 M16 x 60:15',
'High Strength Hex Head Bolt DIN 6914 M16 x 60:15',#33029,#33042,
'High Strength Hex Head Bolt DIN 6914 M16 x 60:15');
#268=NEXT_ASSEMBLY_USAGE_OCCURRENCE(
'High Strength Hex Head Bolt DIN 6914 M16 x 60:16',
'High Strength Hex Head Bolt DIN 6914 M16 x 60:16',
'High Strength Hex Head Bolt DIN 6914 M16 x 60:16',#33029,#33042,
'High Strength Hex Head Bolt DIN 6914 M16 x 60:16');
#269=NEXT_ASSEMBLY_USAGE_OCCURRENCE('Plain Washer DIN 125 A 17:2',
'Plain Washer DIN 125 A 17:2','Plain Washer DIN 125 A 17:2',#33029,#33043,
'Plain Washer DIN 125 A 17:2');
#270=NEXT_ASSEMBLY_USAGE_OCCURRENCE('Plain Washer DIN 125 A 17:3',
'Plain Washer DIN 125 A 17:3','Plain Washer DIN 125 A 17:3',#33029,#33043,
'Plain Washer DIN 125 A 17:3');
#271=NEXT_ASSEMBLY_USAGE_OCCURRENCE('Plain Washer DIN 125 A 17:4',
'Plain Washer DIN 125 A 17:4','Plain Washer DIN 125 A 17:4',#33029,#33043,
'Plain Washer DIN 125 A 17:4');
#272=NEXT_ASSEMBLY_USAGE_OCCURRENCE('Plain Washer DIN 125 A 17:5',
'Plain Washer DIN 125 A 17:5','Plain Washer DIN 125 A 17:5',#33029,#33043,
'Plain Washer DIN 125 A 17:5');
#273=NEXT_ASSEMBLY_USAGE_OCCURRENCE('Plain Washer DIN 125 A 17:6',
'Plain Washer DIN 125 A 17:6','Plain Washer DIN 125 A 17:6',#33029,#33043,
'Plain Washer DIN 125 A 17:6');
#274=NEXT_ASSEMBLY_USAGE_OCCURRENCE('Plain Washer DIN 125 A 17:7',
'Plain Washer DIN 125 A 17:7','Plain Washer DIN 125 A 17:7',#33029,#33043,
'Plain Washer DIN 125 A 17:7');
#275=NEXT_ASSEMBLY_USAGE_OCCURRENCE('Plain Washer DIN 125 A 17:8',
'Plain Washer DIN 125 A 17:8','Plain Washer DIN 125 A 17:8',#33029,#33043,
'Plain Washer DIN 125 A 17:8');
#276=NEXT_ASSEMBLY_USAGE_OCCURRENCE('Plain Washer DIN 125 A 17:9',
'Plain Washer DIN 125 A 17:9','Plain Washer DIN 125 A 17:9',#33029,#33043,
'Plain Washer DIN 125 A 17:9');
#277=NEXT_ASSEMBLY_USAGE_OCCURRENCE('Plain Washer DIN 125 A 17:10',
'Plain Washer DIN 125 A 17:10','Plain Washer DIN 125 A 17:10',#33029,#33043,
'Plain Washer DIN 125 A 17:10');
#278=NEXT_ASSEMBLY_USAGE_OCCURRENCE('Plain Washer DIN 125 A 17:11',
'Plain Washer DIN 125 A 17:11','Plain Washer DIN 125 A 17:11',#33029,#33043,
'Plain Washer DIN 125 A 17:11');
#279=NEXT_ASSEMBLY_USAGE_OCCURRENCE('Plain Washer DIN 125 A 17:12',
'Plain Washer DIN 125 A 17:12','Plain Washer DIN 125 A 17:12',#33029,#33043,
'Plain Washer DIN 125 A 17:12');
#280=NEXT_ASSEMBLY_USAGE_OCCURRENCE('Plain Washer DIN 125 A 17:13',
'Plain Washer DIN 125 A 17:13','Plain Washer DIN 125 A 17:13',#33029,#33043,
'Plain Washer DIN 125 A 17:13');
#281=NEXT_ASSEMBLY_USAGE_OCCURRENCE('Plain Washer DIN 125 A 17:14',
'Plain Washer DIN 125 A 17:14','Plain Washer DIN 125 A 17:14',#33029,#33043,
'Plain Washer DIN 125 A 17:14');
#282=NEXT_ASSEMBLY_USAGE_OCCURRENCE('Plain Washer DIN 125 A 17:15',
'Plain Washer DIN 125 A 17:15','Plain Washer DIN 125 A 17:15',#33029,#33043,
'Plain Washer DIN 125 A 17:15');
#283=NEXT_ASSEMBLY_USAGE_OCCURRENCE('Plain Washer DIN 125 A 17:16',
'Plain Washer DIN 125 A 17:16','Plain Washer DIN 125 A 17:16',#33029,#33043,
'Plain Washer DIN 125 A 17:16');
#284=NEXT_ASSEMBLY_USAGE_OCCURRENCE(
'High Strength Hex Nut DIN 6915 M16:2',
'High Strength Hex Nut DIN 6915 M16:2',
'High Strength Hex Nut DIN 6915 M16:2',#33029,#33044,
'High Strength Hex Nut DIN 6915 M16:2');
#285=NEXT_ASSEMBLY_USAGE_OCCURRENCE(
'High Strength Hex Nut DIN 6915 M16:3',
'High Strength Hex Nut DIN 6915 M16:3',
'High Strength Hex Nut DIN 6915 M16:3',#33029,#33044,
'High Strength Hex Nut DIN 6915 M16:3');
#286=NEXT_ASSEMBLY_USAGE_OCCURRENCE(
'High Strength Hex Nut DIN 6915 M16:4',
'High Strength Hex Nut DIN 6915 M16:4',
'High Strength Hex Nut DIN 6915 M16:4',#33029,#33044,
'High Strength Hex Nut DIN 6915 M16:4');
#287=NEXT_ASSEMBLY_USAGE_OCCURRENCE(
'High Strength Hex Nut DIN 6915 M16:5',
'High Strength Hex Nut DIN 6915 M16:5',
'High Strength Hex Nut DIN 6915 M16:5',#33029,#33044,
'High Strength Hex Nut DIN 6915 M16:5');
#288=NEXT_ASSEMBLY_USAGE_OCCURRENCE(
'High Strength Hex Nut DIN 6915 M16:6',
'High Strength Hex Nut DIN 6915 M16:6',
'High Strength Hex Nut DIN 6915 M16:6',#33029,#33044,
'High Strength Hex Nut DIN 6915 M16:6');
#289=NEXT_ASSEMBLY_USAGE_OCCURRENCE(
'High Strength Hex Nut DIN 6915 M16:7',
'High Strength Hex Nut DIN 6915 M16:7',
'High Strength Hex Nut DIN 6915 M16:7',#33029,#33044,
'High Strength Hex Nut DIN 6915 M16:7');
#290=NEXT_ASSEMBLY_USAGE_OCCURRENCE(
'High Strength Hex Nut DIN 6915 M16:8',
'High Strength Hex Nut DIN 6915 M16:8',
'High Strength Hex Nut DIN 6915 M16:8',#33029,#33044,
'High Strength Hex Nut DIN 6915 M16:8');
#291=NEXT_ASSEMBLY_USAGE_OCCURRENCE(
'High Strength Hex Nut DIN 6915 M16:9',
'High Strength Hex Nut DIN 6915 M16:9',
'High Strength Hex Nut DIN 6915 M16:9',#33029,#33044,
'High Strength Hex Nut DIN 6915 M16:9');
#292=NEXT_ASSEMBLY_USAGE_OCCURRENCE(
'High Strength Hex Nut DIN 6915 M16:10',
'High Strength Hex Nut DIN 6915 M16:10',
'High Strength Hex Nut DIN 6915 M16:10',#33029,#33044,
'High Strength Hex Nut DIN 6915 M16:10');
#293=NEXT_ASSEMBLY_USAGE_OCCURRENCE(
'High Strength Hex Nut DIN 6915 M16:11',
'High Strength Hex Nut DIN 6915 M16:11',
'High Strength Hex Nut DIN 6915 M16:11',#33029,#33044,
'High Strength Hex Nut DIN 6915 M16:11');
#294=NEXT_ASSEMBLY_USAGE_OCCURRENCE(
'High Strength Hex Nut DIN 6915 M16:12',
'High Strength Hex Nut DIN 6915 M16:12',
'High Strength Hex Nut DIN 6915 M16:12',#33029,#33044,
'High Strength Hex Nut DIN 6915 M16:12');
#295=NEXT_ASSEMBLY_USAGE_OCCURRENCE(
'High Strength Hex Nut DIN 6915 M16:13',
'High Strength Hex Nut DIN 6915 M16:13',
'High Strength Hex Nut DIN 6915 M16:13',#33029,#33044,
'High Strength Hex Nut DIN 6915 M16:13');
#296=NEXT_ASSEMBLY_USAGE_OCCURRENCE(
'High Strength Hex Nut DIN 6915 M16:14',
'High Strength Hex Nut DIN 6915 M16:14',
'High Strength Hex Nut DIN 6915 M16:14',#33029,#33044,
'High Strength Hex Nut DIN 6915 M16:14');
#297=NEXT_ASSEMBLY_USAGE_OCCURRENCE(
'High Strength Hex Nut DIN 6915 M16:15',
'High Strength Hex Nut DIN 6915 M16:15',
'High Strength Hex Nut DIN 6915 M16:15',#33029,#33044,
'High Strength Hex Nut DIN 6915 M16:15');
#298=NEXT_ASSEMBLY_USAGE_OCCURRENCE(
'High Strength Hex Nut DIN 6915 M16:16',
'High Strength Hex Nut DIN 6915 M16:16',
'High Strength Hex Nut DIN 6915 M16:16',#33029,#33044,
'High Strength Hex Nut DIN 6915 M16:16');
#299=(
BOUNDED_SURFACE()
B_SPLINE_SURFACE(1,2,((#26568,#26569,#26570,#26571,#26572,#26573,#26574,
#26575,#26576,#26577,#26578,#26579,#26580,#26581,#26582,#26583,#26584,#26585,
#26586,#26587,#26588,#26589,#26590,#26591,#26592,#26593,#26594,#26595,#26596,
#26597,#26598,#26599,#26600,#26601,#26602,#26603,#26604,#26605,#26606,#26607,
#26608,#26609,#26610,#26611,#26612,#26613,#26614,#26615,#26616,#26617,#26618,
#26619,#26620,#26621,#26622,#26623,#26624,#26625,#26626,#26627,#26628,#26629,
#26630,#26631,#26632,#26633,#26634,#26635,#26636,#26637,#26638,#26639,#26640,
#26641,#26642,#26643,#26644,#26645,#26646,#26647,#26648,#26649,#26650,#26651,
#26652,#26653,#26654,#26655,#26656,#26657,#26658,#26659,#26660,#26661,#26662,
#26663,#26664,#26665,#26666,#26667,#26668,#26669,#26670,#26671,#26672,#26673,
#26674,#26675,#26676,#26677,#26678,#26679,#26680,#26681,#26682,#26683,#26684,
#26685,#26686,#26687,#26688,#26689,#26690,#26691,#26692,#26693,#26694,#26695,
#26696,#26697,#26698,#26699,#26700,#26701,#26702,#26703,#26704,#26705,#26706,
#26707,#26708,#26709,#26710,#26711,#26712,#26713,#26714,#26715,#26716,#26717,
#26718,#26719,#26720,#26721,#26722,#26723,#26724,#26725,#26726,#26727,#26728,
#26729,#26730,#26731,#26732,#26733,#26734,#26735,#26736,#26737,#26738,#26739,
#26740,#26741,#26742,#26743,#26744,#26745,#26746,#26747,#26748,#26749,#26750,
#26751,#26752,#26753,#26754,#26755,#26756,#26757,#26758,#26759,#26760,#26761,
#26762,#26763,#26764,#26765,#26766,#26767,#26768,#26769,#26770,#26771,#26772,
#26773,#26774,#26775,#26776,#26777,#26778,#26779,#26780,#26781,#26782,#26783,
#26784,#26785,#26786,#26787,#26788,#26789,#26790,#26791,#26792,#26793,#26794,
#26795,#26796,#26797,#26798,#26799,#26800,#26801,#26802,#26803,#26804,#26805,
#26806,#26807,#26808,#26809,#26810,#26811,#26812,#26813,#26814,#26815,#26816,
#26817,#26818,#26819,#26820,#26821,#26822,#26823,#26824,#26825,#26826,#26827,
#26828,#26829,#26830,#26831,#26832,#26833,#26834,#26835,#26836,#26837,#26838,
#26839,#26840,#26841,#26842,#26843,#26844,#26845,#26846,#26847,#26848,#26849,
#26850,#26851,#26852,#26853,#26854,#26855,#26856,#26857,#26858,#26859,#26860,
#26861,#26862,#26863,#26864,#26865,#26866,#26867,#26868,#26869,#26870,#26871,
#26872,#26873,#26874,#26875,#26876,#26877,#26878,#26879,#26880,#26881,#26882,
#26883,#26884,#26885,#26886,#26887,#26888,#26889,#26890,#26891,#26892,#26893,
#26894,#26895,#26896,#26897,#26898,#26899,#26900,#26901,#26902,#26903,#26904,
#26905,#26906,#26907,#26908,#26909,#26910,#26911,#26912,#26913,#26914,#26915,
#26916,#26917,#26918,#26919,#26920,#26921,#26922,#26923,#26924,#26925,#26926,
#26927,#26928,#26929,#26930,#26931,#26932,#26933,#26934,#26935,#26936,#26937,
#26938,#26939,#26940,#26941,#26942,#26943,#26944,#26945,#26946,#26947,#26948,
#26949,#26950,#26951,#26952,#26953,#26954,#26955,#26956,#26957,#26958,#26959,
#26960,#26961,#26962,#26963,#26964,#26965,#26966,#26967,#26968,#26969,#26970,
#26971,#26972,#26973,#26974,#26975,#26976,#26977,#26978,#26979,#26980,#26981,
#26982,#26983,#26984,#26985,#26986,#26987,#26988,#26989,#26990,#26991,#26992,
#26993,#26994,#26995,#26996,#26997,#26998,#26999,#27000,#27001,#27002,#27003,
#27004),(#27005,#27006,#27007,#27008,#27009,#27010,#27011,#27012,#27013,
#27014,#27015,#27016,#27017,#27018,#27019,#27020,#27021,#27022,#27023,#27024,
#27025,#27026,#27027,#27028,#27029,#27030,#27031,#27032,#27033,#27034,#27035,
#27036,#27037,#27038,#27039,#27040,#27041,#27042,#27043,#27044,#27045,#27046,
#27047,#27048,#27049,#27050,#27051,#27052,#27053,#27054,#27055,#27056,#27057,
#27058,#27059,#27060,#27061,#27062,#27063,#27064,#27065,#27066,#27067,#27068,
#27069,#27070,#27071,#27072,#27073,#27074,#27075,#27076,#27077,#27078,#27079,
#27080,#27081,#27082,#27083,#27084,#27085,#27086,#27087,#27088,#27089,#27090,
#27091,#27092,#27093,#27094,#27095,#27096,#27097,#27098,#27099,#27100,#27101,
#27102,#27103,#27104,#27105,#27106,#27107,#27108,#27109,#27110,#27111,#27112,
#27113,#27114,#27115,#27116,#27117,#27118,#27119,#27120,#27121,#27122,#27123,
#27124,#27125,#27126,#27127,#27128,#27129,#27130,#27131,#27132,#27133,#27134,
#27135,#27136,#27137,#27138,#27139,#27140,#27141,#27142,#27143,#27144,#27145,
#27146,#27147,#27148,#27149,#27150,#27151,#27152,#27153,#27154,#27155,#27156,
#27157,#27158,#27159,#27160,#27161,#27162,#27163,#27164,#27165,#27166,#27167,
#27168,#27169,#27170,#27171,#27172,#27173,#27174,#27175,#27176,#27177,#27178,
#27179,#27180,#27181,#27182,#27183,#27184,#27185,#27186,#27187,#27188,#27189,
#27190,#27191,#27192,#27193,#27194,#27195,#27196,#27197,#27198,#27199,#27200,
#27201,#27202,#27203,#27204,#27205,#27206,#27207,#27208,#27209,#27210,#27211,
#27212,#27213,#27214,#27215,#27216,#27217,#27218,#27219,#27220,#27221,#27222,
#27223,#27224,#27225,#27226,#27227,#27228,#27229,#27230,#27231,#27232,#27233,
#27234,#27235,#27236,#27237,#27238,#27239,#27240,#27241,#27242,#27243,#27244,
#27245,#27246,#27247,#27248,#27249,#27250,#27251,#27252,#27253,#27254,#27255,
#27256,#27257,#27258,#27259,#27260,#27261,#27262,#27263,#27264,#27265,#27266,
#27267,#27268,#27269,#27270,#27271,#27272,#27273,#27274,#27275,#27276,#27277,
#27278,#27279,#27280,#27281,#27282,#27283,#27284,#27285,#27286,#27287,#27288,
#27289,#27290,#27291,#27292,#27293,#27294,#27295,#27296,#27297,#27298,#27299,
#27300,#27301,#27302,#27303,#27304,#27305,#27306,#27307,#27308,#27309,#27310,
#27311,#27312,#27313,#27314,#27315,#27316,#27317,#27318,#27319,#27320,#27321,
#27322,#27323,#27324,#27325,#27326,#27327,#27328,#27329,#27330,#27331,#27332,
#27333,#27334,#27335,#27336,#27337,#27338,#27339,#27340,#27341,#27342,#27343,
#27344,#27345,#27346,#27347,#27348,#27349,#27350,#27351,#27352,#27353,#27354,
#27355,#27356,#27357,#27358,#27359,#27360,#27361,#27362,#27363,#27364,#27365,
#27366,#27367,#27368,#27369,#27370,#27371,#27372,#27373,#27374,#27375,#27376,
#27377,#27378,#27379,#27380,#27381,#27382,#27383,#27384,#27385,#27386,#27387,
#27388,#27389,#27390,#27391,#27392,#27393,#27394,#27395,#27396,#27397,#27398,
#27399,#27400,#27401,#27402,#27403,#27404,#27405,#27406,#27407,#27408,#27409,
#27410,#27411,#27412,#27413,#27414,#27415,#27416,#27417,#27418,#27419,#27420,
#27421,#27422,#27423,#27424,#27425,#27426,#27427,#27428,#27429,#27430,#27431,
#27432,#27433,#27434,#27435,#27436,#27437,#27438,#27439,#27440,#27441)),
 .UNSPECIFIED.,.F.,.F.,.F.)
B_SPLINE_SURFACE_WITH_KNOTS((2,2),(3,2,2,2,2,2,2,2,2,2,2,2,2,2,2,2,2,2,
2,2,2,2,2,2,2,2,2,2,2,2,2,2,2,2,2,2,2,2,2,2,2,2,2,2,2,2,2,2,2,2,2,2,2,2,
2,2,2,2,2,2,2,2,2,2,2,2,2,2,2,2,2,2,2,2,2,2,2,2,2,2,2,2,2,2,2,2,2,2,2,2,
2,2,2,2,2,2,2,2,2,2,2,2,2,2,2,2,2,2,2,2,2,2,2,2,2,2,2,2,2,2,2,2,2,2,2,2,
2,2,2,2,2,2,2,2,2,2,2,2,2,2,2,2,2,2,2,2,2,2,2,2,2,2,2,2,2,2,2,2,2,2,2,2,
2,2,2,2,2,2,2,2,2,2,2,2,2,2,2,2,2,2,2,2,2,2,2,2,2,2,2,2,2,2,2,2,2,2,2,2,
2,2,2,2,2,2,2,2,2,2,2,2,2,2,2,2,2,2,2,2,3),(0.,1.00000935051354),(0.,0.00454545454545455,
0.00909090909090909,0.0136363636363636,0.0181818181818182,0.0227272727272727,
0.0272727272727273,0.0318181818181818,0.0363636363636364,0.0409090909090909,
0.0454545454545455,0.05,0.0545454545454545,0.0590909090909091,0.0636363636363636,
0.0681818181818182,0.0727272727272727,0.0772727272727273,0.0818181818181818,
0.0863636363636364,0.0909090909090909,0.0954545454545455,0.1,0.104545454545455,
0.109090909090909,0.113636363636364,0.118181818181818,0.122727272727273,
0.127272727272727,0.131818181818182,0.136363636363636,0.140909090909091,
0.145454545454545,0.15,0.154545454545455,0.159090909090909,0.163636363636364,
0.168181818181818,0.172727272727273,0.177272727272727,0.181818181818182,
0.186363636363636,0.190909090909091,0.195454545454545,0.2,0.204545454545455,
0.209090909090909,0.213636363636364,0.218181818181818,0.222727272727273,
0.227272727272727,0.231818181818182,0.236363636363636,0.240909090909091,
0.245454545454545,0.25,0.254545454545455,0.259090909090909,0.263636363636364,
0.268181818181818,0.272727272727273,0.277272727272727,0.281818181818182,
0.286363636363636,0.290909090909091,0.295454545454545,0.3,0.304545454545455,
0.309090909090909,0.313636363636364,0.318181818181818,0.322727272727273,
0.327272727272727,0.331818181818182,0.336363636363636,0.340909090909091,
0.345454545454545,0.35,0.354545454545455,0.359090909090909,0.363636363636364,
0.368181818181818,0.372727272727273,0.377272727272727,0.381818181818182,
0.386363636363636,0.390909090909091,0.395454545454545,0.4,0.404545454545455,
0.409090909090909,0.413636363636364,0.418181818181818,0.422727272727273,
0.427272727272727,0.431818181818182,0.436363636363636,0.440909090909091,
0.445454545454545,0.45,0.454545454545455,0.459090909090909,0.463636363636364,
0.468181818181818,0.472727272727273,0.477272727272727,0.481818181818182,
0.486363636363636,0.490909090909091,0.495454545454545,0.5,0.504545454545455,
0.509090909090909,0.513636363636364,0.518181818181818,0.522727272727273,
0.527272727272727,0.531818181818182,0.536363636363636,0.540909090909091,
0.545454545454545,0.55,0.554545454545455,0.559090909090909,0.563636363636364,
0.568181818181818,0.572727272727273,0.577272727272727,0.581818181818182,
0.586363636363636,0.590909090909091,0.595454545454545,0.6,0.604545454545454,
0.609090909090909,0.613636363636364,0.618181818181818,0.622727272727273,
0.627272727272727,0.631818181818182,0.636363636363636,0.640909090909091,
0.645454545454546,0.65,0.654545454545455,0.659090909090909,0.663636363636364,
0.668181818181818,0.672727272727273,0.677272727272727,0.681818181818182,
0.686363636363636,0.690909090909091,0.695454545454545,0.7,0.704545454545455,
0.709090909090909,0.713636363636364,0.718181818181818,0.722727272727273,
0.727272727272727,0.731818181818182,0.736363636363636,0.740909090909091,
0.745454545454545,0.75,0.754545454545455,0.759090909090909,0.763636363636364,
0.768181818181818,0.772727272727273,0.777272727272727,0.781818181818182,
0.786363636363636,0.790909090909091,0.795454545454545,0.8,0.804545454545455,
0.809090909090909,0.813636363636364,0.818181818181818,0.822727272727273,
0.827272727272727,0.831818181818182,0.836363636363636,0.840909090909091,
0.845454545454545,0.85,0.854545454545454,0.859090909090909,0.863636363636364,
0.868181818181818,0.872727272727273,0.877272727272727,0.881818181818182,
0.886363636363636,0.890909090909091,0.895454545454546,0.9,0.904545454545455,
0.909090909090909,0.913636363636364,0.918181818181818,0.922727272727273,
0.927272727272727,0.931818181818182,0.936363636363636,0.940909090909091,
0.945454545454545,0.95,0.954545454545455,0.959090909090909,0.963636363636364,
0.968181818181818,0.972727272727273,0.977272727272727,0.981818181818182,
0.984250640629257,0.99409314703555),.UNSPECIFIED.)
GEOMETRIC_REPRESENTATION_ITEM()
RATIONAL_B_SPLINE_SURFACE(((1.,0.951056516295154,1.,0.951056516295154,1.,
0.951056516295154,1.,0.951056516295154,1.,0.951056516295154,1.,0.951056516295154,
1.,0.951056516295154,1.,0.951056516295154,1.,0.951056516295154,1.,0.951056516295154,
1.,0.951056516295154,1.,0.951056516295154,1.,0.951056516295154,1.,0.951056516295154,
1.,0.951056516295154,1.,0.951056516295154,1.,0.951056516295154,1.,0.951056516295154,
1.,0.951056516295154,1.,0.951056516295154,1.,0.951056516295154,1.,0.951056516295154,
1.,0.951056516295154,1.,0.951056516295154,1.,0.951056516295154,1.,0.951056516295154,
1.,0.951056516295154,1.,0.951056516295154,1.,0.951056516295154,1.,0.951056516295154,
1.,0.951056516295154,1.,0.951056516295154,1.,0.951056516295154,1.,0.951056516295154,
1.,0.951056516295154,1.,0.951056516295154,1.,0.951056516295154,1.,0.951056516295154,
1.,0.951056516295154,1.,0.951056516295154,1.,0.951056516295154,1.,0.951056516295154,
1.,0.951056516295154,1.,0.951056516295154,1.,0.951056516295154,1.,0.951056516295154,
1.,0.951056516295154,1.,0.951056516295154,1.,0.951056516295154,1.,0.951056516295154,
1.,0.951056516295154,1.,0.951056516295154,1.,0.951056516295154,1.,0.951056516295154,
1.,0.951056516295154,1.,0.951056516295154,1.,0.951056516295154,1.,0.951056516295154,
1.,0.951056516295154,1.,0.951056516295154,1.,0.951056516295154,1.,0.951056516295154,
1.,0.951056516295154,1.,0.951056516295154,1.,0.951056516295154,1.,0.951056516295154,
1.,0.951056516295154,1.,0.951056516295154,1.,0.951056516295154,1.,0.951056516295154,
1.,0.951056516295154,1.,0.951056516295154,1.,0.951056516295154,1.,0.951056516295154,
1.,0.951056516295154,1.,0.951056516295154,1.,0.951056516295154,1.,0.951056516295154,
1.,0.951056516295154,1.,0.951056516295154,1.,0.951056516295154,1.,0.951056516295154,
1.,0.951056516295154,1.,0.951056516295154,1.,0.951056516295154,1.,0.951056516295154,
1.,0.951056516295154,1.,0.951056516295154,1.,0.951056516295154,1.,0.951056516295154,
1.,0.951056516295154,1.,0.951056516295154,1.,0.951056516295154,1.,0.951056516295154,
1.,0.951056516295154,1.,0.951056516295154,1.,0.951056516295154,1.,0.951056516295154,
1.,0.951056516295154,1.,0.951056516295154,1.,0.951056516295154,1.,0.951056516295154,
1.,0.951056516295154,1.,0.951056516295154,1.,0.951056516295154,1.,0.951056516295154,
1.,0.951056516295154,1.,0.951056516295154,1.,0.951056516295154,1.,0.951056516295154,
1.,0.951056516295154,1.,0.951056516295154,1.,0.951056516295154,1.,0.951056516295154,
1.,0.951056516295154,1.,0.951056516295154,1.,0.951056516295154,1.,0.951056516295154,
1.,0.951056516295154,1.,0.951056516295154,1.,0.951056516295154,1.,0.951056516295154,
1.,0.951056516295154,1.,0.951056516295154,1.,0.951056516295154,1.,0.951056516295154,
1.,0.951056516295154,1.,0.951056516295154,1.,0.951056516295154,1.,0.951056516295154,
1.,0.951056516295154,1.,0.951056516295154,1.,0.951056516295154,1.,0.951056516295154,
1.,0.951056516295154,1.,0.951056516295154,1.,0.951056516295154,1.,0.951056516295154,
1.,0.951056516295154,1.,0.951056516295154,1.,0.951056516295154,1.,0.951056516295154,
1.,0.951056516295154,1.,0.951056516295154,1.,0.951056516295154,1.,0.951056516295154,
1.,0.951056516295154,1.,0.951056516295154,1.,0.951056516295154,1.,0.951056516295154,
1.,0.951056516295154,1.,0.951056516295154,1.,0.951056516295154,1.,0.951056516295154,
1.,0.951056516295154,1.,0.951056516295154,1.,0.951056516295154,1.,0.951056516295154,
1.,0.951056516295154,1.,0.951056516295154,1.,0.951056516295154,1.,0.951056516295154,
1.,0.951056516295154,1.,0.951056516295154,1.,0.951056516295154,1.,0.951056516295154,
1.,0.951056516295154,1.,0.951056516295154,1.,0.951056516295154,1.,0.951056516295154,
1.,0.951056516295154,1.,0.951056516295154,1.,0.951056516295154,1.,0.951056516295154,
1.,0.951056516295154,1.,0.951056516295154,1.,0.951056516295154,1.,0.951056516295154,
1.,0.951056516295154,1.,0.951056516295154,1.,0.951056516295154,1.,0.951056516295154,
1.,0.951056516295154,1.,0.951056516295154,1.,0.951056516295154,1.,0.951056516295154,
1.,0.951056516295154,1.,0.951056516295154,1.,0.951056516295154,1.,0.951056516295154,
1.,0.951056516295154,1.,0.951056516295154,1.,0.951056516295154,1.,0.951056516295154,
1.,0.951056516295154,1.,0.951056516295154,1.,0.951056516295154,1.,0.951056516295154,
1.,0.951056516295154,1.,0.951056516295154,1.,0.951056516295154,1.,0.951056516295154,
1.,0.951056516295154,1.,0.951056516295154,1.,0.951056516295154,1.,0.951056516295154,
1.,0.951056516295154,1.,0.951056516295154,1.,0.951056516295154,1.,0.951056516295154,
1.,0.951056516295154,1.,0.951056516295154,1.,0.951056516295154,1.,0.951056516295154,
1.,0.951056516295154,1.,0.951056516295154,1.,0.973808338199829,0.975649137349576,
0.975649137349576,0.975649137349576),(1.,0.951056516295154,1.,0.951056516295154,
1.,0.951056516295154,1.,0.951056516295154,1.,0.951056516295154,1.,0.951056516295154,
1.,0.951056516295154,1.,0.951056516295154,1.,0.951056516295154,1.,0.951056516295154,
1.,0.951056516295154,1.,0.951056516295154,1.,0.951056516295154,1.,0.951056516295154,
1.,0.951056516295154,1.,0.951056516295154,1.,0.951056516295154,1.,0.951056516295154,
1.,0.951056516295154,1.,0.951056516295154,1.,0.951056516295154,1.,0.951056516295154,
1.,0.951056516295154,1.,0.951056516295154,1.,0.951056516295154,1.,0.951056516295154,
1.,0.951056516295154,1.,0.951056516295154,1.,0.951056516295154,1.,0.951056516295154,
1.,0.951056516295154,1.,0.951056516295154,1.,0.951056516295154,1.,0.951056516295154,
1.,0.951056516295154,1.,0.951056516295154,1.,0.951056516295154,1.,0.951056516295154,
1.,0.951056516295154,1.,0.951056516295154,1.,0.951056516295154,1.,0.951056516295154,
1.,0.951056516295154,1.,0.951056516295154,1.,0.951056516295154,1.,0.951056516295154,
1.,0.951056516295154,1.,0.951056516295154,1.,0.951056516295154,1.,0.951056516295154,
1.,0.951056516295154,1.,0.951056516295154,1.,0.951056516295154,1.,0.951056516295154,
1.,0.951056516295154,1.,0.951056516295154,1.,0.951056516295154,1.,0.951056516295154,
1.,0.951056516295154,1.,0.951056516295154,1.,0.951056516295154,1.,0.951056516295154,
1.,0.951056516295154,1.,0.951056516295154,1.,0.951056516295154,1.,0.951056516295154,
1.,0.951056516295154,1.,0.951056516295154,1.,0.951056516295154,1.,0.951056516295154,
1.,0.951056516295154,1.,0.951056516295154,1.,0.951056516295154,1.,0.951056516295154,
1.,0.951056516295154,1.,0.951056516295154,1.,0.951056516295154,1.,0.951056516295154,
1.,0.951056516295154,1.,0.951056516295154,1.,0.951056516295154,1.,0.951056516295154,
1.,0.951056516295154,1.,0.951056516295154,1.,0.951056516295154,1.,0.951056516295154,
1.,0.951056516295154,1.,0.951056516295154,1.,0.951056516295154,1.,0.951056516295154,
1.,0.951056516295154,1.,0.951056516295154,1.,0.951056516295154,1.,0.951056516295154,
1.,0.951056516295154,1.,0.951056516295154,1.,0.951056516295154,1.,0.951056516295154,
1.,0.951056516295154,1.,0.951056516295154,1.,0.951056516295154,1.,0.951056516295154,
1.,0.951056516295154,1.,0.951056516295154,1.,0.951056516295154,1.,0.951056516295154,
1.,0.951056516295154,1.,0.951056516295154,1.,0.951056516295154,1.,0.951056516295154,
1.,0.951056516295154,1.,0.951056516295154,1.,0.951056516295154,1.,0.951056516295154,
1.,0.951056516295154,1.,0.951056516295154,1.,0.951056516295154,1.,0.951056516295154,
1.,0.951056516295154,1.,0.951056516295154,1.,0.951056516295154,1.,0.951056516295154,
1.,0.951056516295154,1.,0.951056516295154,1.,0.951056516295154,1.,0.951056516295154,
1.,0.951056516295154,1.,0.951056516295154,1.,0.951056516295154,1.,0.951056516295154,
1.,0.951056516295154,1.,0.951056516295154,1.,0.951056516295154,1.,0.951056516295154,
1.,0.951056516295154,1.,0.951056516295154,1.,0.951056516295154,1.,0.951056516295154,
1.,0.951056516295154,1.,0.951056516295154,1.,0.951056516295154,1.,0.951056516295154,
1.,0.951056516295154,1.,0.951056516295154,1.,0.951056516295154,1.,0.951056516295154,
1.,0.951056516295154,1.,0.951056516295154,1.,0.951056516295154,1.,0.951056516295154,
1.,0.951056516295154,1.,0.951056516295154,1.,0.951056516295154,1.,0.951056516295154,
1.,0.951056516295154,1.,0.951056516295154,1.,0.951056516295154,1.,0.951056516295154,
1.,0.951056516295154,1.,0.951056516295154,1.,0.951056516295154,1.,0.951056516295154,
1.,0.951056516295154,1.,0.951056516295154,1.,0.951056516295154,1.,0.951056516295154,
1.,0.951056516295154,1.,0.951056516295154,1.,0.951056516295154,1.,0.951056516295154,
1.,0.951056516295154,1.,0.951056516295154,1.,0.951056516295154,1.,0.951056516295154,
1.,0.951056516295154,1.,0.951056516295154,1.,0.951056516295154,1.,0.951056516295154,
1.,0.951056516295154,1.,0.951056516295154,1.,0.951056516295154,1.,0.951056516295154,
1.,0.951056516295154,1.,0.951056516295154,1.,0.951056516295154,1.,0.951056516295154,
1.,0.951056516295154,1.,0.951056516295154,1.,0.951056516295154,1.,0.951056516295154,
1.,0.951056516295154,1.,0.951056516295154,1.,0.951056516295154,1.,0.951056516295154,
1.,0.951056516295154,1.,0.951056516295154,1.,0.951056516295154,1.,0.951056516295154,
1.,0.951056516295154,1.,0.951056516295154,1.,0.951056516295154,1.,0.951056516295154,
1.,0.951056516295154,1.,0.951056516295154,1.,0.951056516295154,1.,0.951056516295154,
1.,0.951056516295154,1.,0.951056516295154,1.,0.951056516295154,1.,0.951056516295154,
1.,0.951056516295154,1.,0.951056516295154,1.,0.951056516295154,1.,0.951056516295154,
1.,0.951056516295154,1.,0.951056516295154,1.,0.973808338199829,0.975649137349576,
0.975649137349576,0.975649137349576)))
REPRESENTATION_ITEM('')
SURFACE()
);
#300=(
BOUNDED_SURFACE()
B_SPLINE_SURFACE(1,2,((#27453,#27454,#27455,#27456,#27457,#27458,#27459,
#27460,#27461,#27462,#27463,#27464,#27465,#27466,#27467,#27468,#27469,#27470,
#27471,#27472,#27473,#27474,#27475,#27476,#27477,#27478,#27479,#27480,#27481,
#27482,#27483,#27484,#27485,#27486,#27487,#27488,#27489,#27490,#27491,#27492,
#27493,#27494,#27495,#27496,#27497,#27498,#27499,#27500,#27501,#27502,#27503,
#27504,#27505,#27506,#27507,#27508,#27509,#27510,#27511,#27512,#27513,#27514,
#27515,#27516,#27517,#27518,#27519,#27520,#27521,#27522,#27523,#27524,#27525,
#27526,#27527,#27528,#27529,#27530,#27531,#27532,#27533,#27534,#27535,#27536,
#27537,#27538,#27539,#27540,#27541,#27542,#27543,#27544,#27545,#27546,#27547,
#27548,#27549,#27550,#27551,#27552,#27553,#27554,#27555,#27556,#27557,#27558,
#27559,#27560,#27561,#27562,#27563,#27564,#27565,#27566,#27567,#27568,#27569,
#27570,#27571,#27572,#27573,#27574,#27575,#27576,#27577,#27578,#27579,#27580,
#27581,#27582,#27583,#27584,#27585,#27586,#27587,#27588,#27589,#27590,#27591,
#27592,#27593,#27594,#27595,#27596,#27597,#27598,#27599,#27600,#27601,#27602,
#27603,#27604,#27605,#27606,#27607,#27608,#27609,#27610,#27611,#27612,#27613,
#27614,#27615,#27616,#27617,#27618,#27619,#27620,#27621,#27622,#27623,#27624,
#27625,#27626,#27627,#27628,#27629,#27630,#27631,#27632,#27633,#27634,#27635,
#27636,#27637,#27638,#27639,#27640,#27641,#27642,#27643,#27644,#27645,#27646,
#27647,#27648,#27649,#27650,#27651,#27652,#27653,#27654,#27655,#27656,#27657,
#27658,#27659,#27660,#27661,#27662,#27663,#27664,#27665,#27666,#27667,#27668,
#27669,#27670,#27671,#27672,#27673,#27674,#27675,#27676,#27677,#27678,#27679,
#27680,#27681,#27682,#27683,#27684,#27685,#27686,#27687,#27688,#27689,#27690,
#27691,#27692,#27693,#27694,#27695,#27696,#27697,#27698,#27699,#27700,#27701,
#27702,#27703,#27704,#27705,#27706,#27707,#27708,#27709,#27710,#27711,#27712,
#27713,#27714,#27715,#27716,#27717,#27718,#27719,#27720,#27721,#27722,#27723,
#27724,#27725,#27726,#27727,#27728,#27729,#27730,#27731,#27732,#27733,#27734,
#27735,#27736,#27737,#27738,#27739,#27740,#27741,#27742,#27743,#27744,#27745,
#27746,#27747,#27748,#27749,#27750,#27751,#27752,#27753,#27754,#27755,#27756,
#27757,#27758,#27759,#27760,#27761,#27762,#27763,#27764,#27765,#27766,#27767,
#27768,#27769,#27770,#27771,#27772,#27773,#27774,#27775,#27776,#27777,#27778,
#27779,#27780,#27781,#27782,#27783,#27784,#27785,#27786,#27787,#27788,#27789,
#27790,#27791,#27792,#27793,#27794,#27795,#27796,#27797,#27798,#27799,#27800,
#27801,#27802,#27803,#27804,#27805,#27806,#27807,#27808,#27809,#27810,#27811,
#27812,#27813,#27814,#27815,#27816,#27817,#27818,#27819,#27820,#27821,#27822,
#27823,#27824,#27825,#27826,#27827,#27828,#27829,#27830,#27831,#27832,#27833,
#27834,#27835,#27836,#27837,#27838,#27839,#27840,#27841,#27842,#27843,#27844,
#27845,#27846,#27847,#27848,#27849,#27850,#27851,#27852,#27853,#27854,#27855,
#27856,#27857,#27858,#27859,#27860,#27861,#27862,#27863,#27864,#27865,#27866,
#27867,#27868,#27869,#27870,#27871,#27872,#27873,#27874,#27875,#27876,#27877,
#27878,#27879,#27880,#27881,#27882,#27883,#27884,#27885,#27886,#27887),
(#27888,#27889,#27890,#27891,#27892,#27893,#27894,#27895,#27896,#27897,
#27898,#27899,#27900,#27901,#27902,#27903,#27904,#27905,#27906,#27907,#27908,
#27909,#27910,#27911,#27912,#27913,#27914,#27915,#27916,#27917,#27918,#27919,
#27920,#27921,#27922,#27923,#27924,#27925,#27926,#27927,#27928,#27929,#27930,
#27931,#27932,#27933,#27934,#27935,#27936,#27937,#27938,#27939,#27940,#27941,
#27942,#27943,#27944,#27945,#27946,#27947,#27948,#27949,#27950,#27951,#27952,
#27953,#27954,#27955,#27956,#27957,#27958,#27959,#27960,#27961,#27962,#27963,
#27964,#27965,#27966,#27967,#27968,#27969,#27970,#27971,#27972,#27973,#27974,
#27975,#27976,#27977,#27978,#27979,#27980,#27981,#27982,#27983,#27984,#27985,
#27986,#27987,#27988,#27989,#27990,#27991,#27992,#27993,#27994,#27995,#27996,
#27997,#27998,#27999,#28000,#28001,#28002,#28003,#28004,#28005,#28006,#28007,
#28008,#28009,#28010,#28011,#28012,#28013,#28014,#28015,#28016,#28017,#28018,
#28019,#28020,#28021,#28022,#28023,#28024,#28025,#28026,#28027,#28028,#28029,
#28030,#28031,#28032,#28033,#28034,#28035,#28036,#28037,#28038,#28039,#28040,
#28041,#28042,#28043,#28044,#28045,#28046,#28047,#28048,#28049,#28050,#28051,
#28052,#28053,#28054,#28055,#28056,#28057,#28058,#28059,#28060,#28061,#28062,
#28063,#28064,#28065,#28066,#28067,#28068,#28069,#28070,#28071,#28072,#28073,
#28074,#28075,#28076,#28077,#28078,#28079,#28080,#28081,#28082,#28083,#28084,
#28085,#28086,#28087,#28088,#28089,#28090,#28091,#28092,#28093,#28094,#28095,
#28096,#28097,#28098,#28099,#28100,#28101,#28102,#28103,#28104,#28105,#28106,
#28107,#28108,#28109,#28110,#28111,#28112,#28113,#28114,#28115,#28116,#28117,
#28118,#28119,#28120,#28121,#28122,#28123,#28124,#28125,#28126,#28127,#28128,
#28129,#28130,#28131,#28132,#28133,#28134,#28135,#28136,#28137,#28138,#28139,
#28140,#28141,#28142,#28143,#28144,#28145,#28146,#28147,#28148,#28149,#28150,
#28151,#28152,#28153,#28154,#28155,#28156,#28157,#28158,#28159,#28160,#28161,
#28162,#28163,#28164,#28165,#28166,#28167,#28168,#28169,#28170,#28171,#28172,
#28173,#28174,#28175,#28176,#28177,#28178,#28179,#28180,#28181,#28182,#28183,
#28184,#28185,#28186,#28187,#28188,#28189,#28190,#28191,#28192,#28193,#28194,
#28195,#28196,#28197,#28198,#28199,#28200,#28201,#28202,#28203,#28204,#28205,
#28206,#28207,#28208,#28209,#28210,#28211,#28212,#28213,#28214,#28215,#28216,
#28217,#28218,#28219,#28220,#28221,#28222,#28223,#28224,#28225,#28226,#28227,
#28228,#28229,#28230,#28231,#28232,#28233,#28234,#28235,#28236,#28237,#28238,
#28239,#28240,#28241,#28242,#28243,#28244,#28245,#28246,#28247,#28248,#28249,
#28250,#28251,#28252,#28253,#28254,#28255,#28256,#28257,#28258,#28259,#28260,
#28261,#28262,#28263,#28264,#28265,#28266,#28267,#28268,#28269,#28270,#28271,
#28272,#28273,#28274,#28275,#28276,#28277,#28278,#28279,#28280,#28281,#28282,
#28283,#28284,#28285,#28286,#28287,#28288,#28289,#28290,#28291,#28292,#28293,
#28294,#28295,#28296,#28297,#28298,#28299,#28300,#28301,#28302,#28303,#28304,
#28305,#28306,#28307,#28308,#28309,#28310,#28311,#28312,#28313,#28314,#28315,
#28316,#28317,#28318,#28319,#28320,#28321,#28322)),.UNSPECIFIED.,.F.,.F.,
 .F.)
B_SPLINE_SURFACE_WITH_KNOTS((2,2),(3,2,2,2,2,2,2,2,2,2,2,2,2,2,2,2,2,2,
2,2,2,2,2,2,2,2,2,2,2,2,2,2,2,2,2,2,2,2,2,2,2,2,2,2,2,2,2,2,2,2,2,2,2,2,
2,2,2,2,2,2,2,2,2,2,2,2,2,2,2,2,2,2,2,2,2,2,2,2,2,2,2,2,2,2,2,2,2,2,2,2,
2,2,2,2,2,2,2,2,2,2,2,2,2,2,2,2,2,2,2,2,2,2,2,2,2,2,2,2,2,2,2,2,2,2,2,2,
2,2,2,2,2,2,2,2,2,2,2,2,2,2,2,2,2,2,2,2,2,2,2,2,2,2,2,2,2,2,2,2,2,2,2,2,
2,2,2,2,2,2,2,2,2,2,2,2,2,2,2,2,2,2,2,2,2,2,2,2,2,2,2,2,2,2,2,2,2,2,2,2,
2,2,2,2,2,2,2,2,2,2,2,2,2,2,2,2,2,2,2,3),(0.,1.),(0.,0.00454545454545455,
0.00909090909090909,0.0136363636363636,0.0181818181818182,0.0227272727272727,
0.0272727272727273,0.0318181818181818,0.0363636363636364,0.0409090909090909,
0.0454545454545455,0.05,0.0545454545454545,0.0590909090909091,0.0636363636363636,
0.0681818181818182,0.0727272727272727,0.0772727272727273,0.0818181818181818,
0.0863636363636364,0.0909090909090909,0.0954545454545455,0.1,0.104545454545455,
0.109090909090909,0.113636363636364,0.118181818181818,0.122727272727273,
0.127272727272727,0.131818181818182,0.136363636363636,0.140909090909091,
0.145454545454545,0.15,0.154545454545455,0.159090909090909,0.163636363636364,
0.168181818181818,0.172727272727273,0.177272727272727,0.181818181818182,
0.186363636363636,0.190909090909091,0.195454545454545,0.2,0.204545454545455,
0.209090909090909,0.213636363636364,0.218181818181818,0.222727272727273,
0.227272727272727,0.231818181818182,0.236363636363636,0.240909090909091,
0.245454545454545,0.25,0.254545454545455,0.259090909090909,0.263636363636364,
0.268181818181818,0.272727272727273,0.277272727272727,0.281818181818182,
0.286363636363636,0.290909090909091,0.295454545454545,0.3,0.304545454545455,
0.309090909090909,0.313636363636364,0.318181818181818,0.322727272727273,
0.327272727272727,0.331818181818182,0.336363636363636,0.340909090909091,
0.345454545454545,0.35,0.354545454545455,0.359090909090909,0.363636363636364,
0.368181818181818,0.372727272727273,0.377272727272727,0.381818181818182,
0.386363636363636,0.390909090909091,0.395454545454545,0.4,0.404545454545455,
0.409090909090909,0.413636363636364,0.418181818181818,0.422727272727273,
0.427272727272727,0.431818181818182,0.436363636363636,0.440909090909091,
0.445454545454545,0.45,0.454545454545455,0.459090909090909,0.463636363636364,
0.468181818181818,0.472727272727273,0.477272727272727,0.481818181818182,
0.486363636363636,0.490909090909091,0.495454545454545,0.5,0.504545454545455,
0.509090909090909,0.513636363636364,0.518181818181818,0.522727272727273,
0.527272727272727,0.531818181818182,0.536363636363636,0.540909090909091,
0.545454545454545,0.55,0.554545454545455,0.559090909090909,0.563636363636364,
0.568181818181818,0.572727272727273,0.577272727272727,0.581818181818182,
0.586363636363636,0.590909090909091,0.595454545454545,0.6,0.604545454545454,
0.609090909090909,0.613636363636364,0.618181818181818,0.622727272727273,
0.627272727272727,0.631818181818182,0.636363636363636,0.640909090909091,
0.645454545454546,0.65,0.654545454545455,0.659090909090909,0.663636363636364,
0.668181818181818,0.672727272727273,0.677272727272727,0.681818181818182,
0.686363636363636,0.690909090909091,0.695454545454545,0.7,0.704545454545455,
0.709090909090909,0.713636363636364,0.718181818181818,0.722727272727273,
0.727272727272727,0.731818181818182,0.736363636363636,0.740909090909091,
0.745454545454545,0.75,0.754545454545455,0.759090909090909,0.763636363636364,
0.768181818181818,0.772727272727273,0.777272727272727,0.781818181818182,
0.786363636363636,0.790909090909091,0.795454545454545,0.8,0.804545454545455,
0.809090909090909,0.813636363636364,0.818181818181818,0.822727272727273,
0.827272727272727,0.831818181818182,0.836363636363636,0.840909090909091,
0.845454545454545,0.85,0.854545454545454,0.859090909090909,0.863636363636364,
0.868181818181818,0.872727272727273,0.877272727272727,0.881818181818182,
0.886363636363636,0.890909090909091,0.895454545454546,0.9,0.904545454545455,
0.909090909090909,0.913636363636364,0.918181818181818,0.922727272727273,
0.927272727272727,0.931818181818182,0.936363636363636,0.940909090909091,
0.945454545454545,0.95,0.954545454545455,0.959090909090909,0.963636363636364,
0.968181818181818,0.972727272727273,0.977272727272727,0.981818181818182,
0.984250643037892),.UNSPECIFIED.)
GEOMETRIC_REPRESENTATION_ITEM()
RATIONAL_B_SPLINE_SURFACE(((1.,0.951056516295154,1.,0.951056516295154,1.,
0.951056516295154,1.,0.951056516295154,1.,0.951056516295154,1.,0.951056516295154,
1.,0.951056516295154,1.,0.951056516295154,1.,0.951056516295154,1.,0.951056516295154,
1.,0.951056516295154,1.,0.951056516295154,1.,0.951056516295154,1.,0.951056516295154,
1.,0.951056516295154,1.,0.951056516295154,1.,0.951056516295154,1.,0.951056516295154,
1.,0.951056516295154,1.,0.951056516295154,1.,0.951056516295154,1.,0.951056516295154,
1.,0.951056516295154,1.,0.951056516295154,1.,0.951056516295154,1.,0.951056516295154,
1.,0.951056516295154,1.,0.951056516295154,1.,0.951056516295154,1.,0.951056516295154,
1.,0.951056516295154,1.,0.951056516295154,1.,0.951056516295154,1.,0.951056516295154,
1.,0.951056516295154,1.,0.951056516295154,1.,0.951056516295154,1.,0.951056516295154,
1.,0.951056516295154,1.,0.951056516295154,1.,0.951056516295154,1.,0.951056516295154,
1.,0.951056516295154,1.,0.951056516295154,1.,0.951056516295154,1.,0.951056516295154,
1.,0.951056516295154,1.,0.951056516295154,1.,0.951056516295154,1.,0.951056516295154,
1.,0.951056516295154,1.,0.951056516295154,1.,0.951056516295154,1.,0.951056516295154,
1.,0.951056516295154,1.,0.951056516295154,1.,0.951056516295154,1.,0.951056516295154,
1.,0.951056516295154,1.,0.951056516295154,1.,0.951056516295154,1.,0.951056516295154,
1.,0.951056516295154,1.,0.951056516295154,1.,0.951056516295154,1.,0.951056516295154,
1.,0.951056516295154,1.,0.951056516295154,1.,0.951056516295154,1.,0.951056516295154,
1.,0.951056516295154,1.,0.951056516295154,1.,0.951056516295154,1.,0.951056516295154,
1.,0.951056516295154,1.,0.951056516295154,1.,0.951056516295154,1.,0.951056516295154,
1.,0.951056516295154,1.,0.951056516295154,1.,0.951056516295154,1.,0.951056516295154,
1.,0.951056516295154,1.,0.951056516295154,1.,0.951056516295154,1.,0.951056516295154,
1.,0.951056516295154,1.,0.951056516295154,1.,0.951056516295154,1.,0.951056516295154,
1.,0.951056516295154,1.,0.951056516295154,1.,0.951056516295154,1.,0.951056516295154,
1.,0.951056516295154,1.,0.951056516295154,1.,0.951056516295154,1.,0.951056516295154,
1.,0.951056516295154,1.,0.951056516295154,1.,0.951056516295154,1.,0.951056516295154,
1.,0.951056516295154,1.,0.951056516295154,1.,0.951056516295154,1.,0.951056516295154,
1.,0.951056516295154,1.,0.951056516295154,1.,0.951056516295154,1.,0.951056516295154,
1.,0.951056516295154,1.,0.951056516295154,1.,0.951056516295154,1.,0.951056516295154,
1.,0.951056516295154,1.,0.951056516295154,1.,0.951056516295154,1.,0.951056516295154,
1.,0.951056516295154,1.,0.951056516295154,1.,0.951056516295154,1.,0.951056516295154,
1.,0.951056516295154,1.,0.951056516295154,1.,0.951056516295154,1.,0.951056516295154,
1.,0.951056516295154,1.,0.951056516295154,1.,0.951056516295154,1.,0.951056516295154,
1.,0.951056516295154,1.,0.951056516295154,1.,0.951056516295154,1.,0.951056516295154,
1.,0.951056516295154,1.,0.951056516295154,1.,0.951056516295154,1.,0.951056516295154,
1.,0.951056516295154,1.,0.951056516295154,1.,0.951056516295154,1.,0.951056516295154,
1.,0.951056516295154,1.,0.951056516295154,1.,0.951056516295154,1.,0.951056516295154,
1.,0.951056516295154,1.,0.951056516295154,1.,0.951056516295154,1.,0.951056516295154,
1.,0.951056516295154,1.,0.951056516295154,1.,0.951056516295154,1.,0.951056516295154,
1.,0.951056516295154,1.,0.951056516295154,1.,0.951056516295154,1.,0.951056516295154,
1.,0.951056516295154,1.,0.951056516295154,1.,0.951056516295154,1.,0.951056516295154,
1.,0.951056516295154,1.,0.951056516295154,1.,0.951056516295154,1.,0.951056516295154,
1.,0.951056516295154,1.,0.951056516295154,1.,0.951056516295154,1.,0.951056516295154,
1.,0.951056516295154,1.,0.951056516295154,1.,0.951056516295154,1.,0.951056516295154,
1.,0.951056516295154,1.,0.951056516295154,1.,0.951056516295154,1.,0.951056516295154,
1.,0.951056516295154,1.,0.951056516295154,1.,0.951056516295154,1.,0.951056516295154,
1.,0.951056516295154,1.,0.951056516295154,1.,0.951056516295154,1.,0.951056516295154,
1.,0.951056516295154,1.,0.951056516295154,1.,0.951056516295154,1.,0.951056516295154,
1.,0.951056516295154,1.,0.951056516295154,1.,0.951056516295154,1.,0.951056516295154,
1.,0.951056516295154,1.,0.951056516295154,1.,0.951056516295154,1.,0.951056516295154,
1.,0.951056516295154,1.,0.951056516295154,1.,0.951056516295154,1.,0.951056516295154,
1.,0.951056516295154,1.,0.951056516295154,1.,0.951056516295154,1.,0.951056516295154,
1.,0.951056516295154,1.,0.951056516295154,1.,0.951056516295154,1.,0.951056516295154,
1.,0.951056516295154,1.,0.951056516295154,1.,0.951056516295154,1.,0.951056516295154,
1.,0.951056516295154,1.,0.951056516295154,1.,0.973808312264696,0.975649140995143),
(1.,0.951056516295154,1.,0.951056516295154,1.,0.951056516295154,1.,0.951056516295154,
1.,0.951056516295154,1.,0.951056516295154,1.,0.951056516295154,1.,0.951056516295154,
1.,0.951056516295154,1.,0.951056516295154,1.,0.951056516295154,1.,0.951056516295154,
1.,0.951056516295154,1.,0.951056516295154,1.,0.951056516295154,1.,0.951056516295154,
1.,0.951056516295154,1.,0.951056516295154,1.,0.951056516295154,1.,0.951056516295154,
1.,0.951056516295154,1.,0.951056516295154,1.,0.951056516295154,1.,0.951056516295154,
1.,0.951056516295154,1.,0.951056516295154,1.,0.951056516295154,1.,0.951056516295154,
1.,0.951056516295154,1.,0.951056516295154,1.,0.951056516295154,1.,0.951056516295154,
1.,0.951056516295154,1.,0.951056516295154,1.,0.951056516295154,1.,0.951056516295154,
1.,0.951056516295154,1.,0.951056516295154,1.,0.951056516295154,1.,0.951056516295154,
1.,0.951056516295154,1.,0.951056516295154,1.,0.951056516295154,1.,0.951056516295154,
1.,0.951056516295154,1.,0.951056516295154,1.,0.951056516295154,1.,0.951056516295154,
1.,0.951056516295154,1.,0.951056516295154,1.,0.951056516295154,1.,0.951056516295154,
1.,0.951056516295154,1.,0.951056516295154,1.,0.951056516295154,1.,0.951056516295154,
1.,0.951056516295154,1.,0.951056516295154,1.,0.951056516295154,1.,0.951056516295154,
1.,0.951056516295154,1.,0.951056516295154,1.,0.951056516295154,1.,0.951056516295154,
1.,0.951056516295154,1.,0.951056516295154,1.,0.951056516295154,1.,0.951056516295154,
1.,0.951056516295154,1.,0.951056516295154,1.,0.951056516295154,1.,0.951056516295154,
1.,0.951056516295154,1.,0.951056516295154,1.,0.951056516295154,1.,0.951056516295154,
1.,0.951056516295154,1.,0.951056516295154,1.,0.951056516295154,1.,0.951056516295154,
1.,0.951056516295154,1.,0.951056516295154,1.,0.951056516295154,1.,0.951056516295154,
1.,0.951056516295154,1.,0.951056516295154,1.,0.951056516295154,1.,0.951056516295154,
1.,0.951056516295154,1.,0.951056516295154,1.,0.951056516295154,1.,0.951056516295154,
1.,0.951056516295154,1.,0.951056516295154,1.,0.951056516295154,1.,0.951056516295154,
1.,0.951056516295154,1.,0.951056516295154,1.,0.951056516295154,1.,0.951056516295154,
1.,0.951056516295154,1.,0.951056516295154,1.,0.951056516295154,1.,0.951056516295154,
1.,0.951056516295154,1.,0.951056516295154,1.,0.951056516295154,1.,0.951056516295154,
1.,0.951056516295154,1.,0.951056516295154,1.,0.951056516295154,1.,0.951056516295154,
1.,0.951056516295154,1.,0.951056516295154,1.,0.951056516295154,1.,0.951056516295154,
1.,0.951056516295154,1.,0.951056516295154,1.,0.951056516295154,1.,0.951056516295154,
1.,0.951056516295154,1.,0.951056516295154,1.,0.951056516295154,1.,0.951056516295154,
1.,0.951056516295154,1.,0.951056516295154,1.,0.951056516295154,1.,0.951056516295154,
1.,0.951056516295154,1.,0.951056516295154,1.,0.951056516295154,1.,0.951056516295154,
1.,0.951056516295154,1.,0.951056516295154,1.,0.951056516295154,1.,0.951056516295154,
1.,0.951056516295154,1.,0.951056516295154,1.,0.951056516295154,1.,0.951056516295154,
1.,0.951056516295154,1.,0.951056516295154,1.,0.951056516295154,1.,0.951056516295154,
1.,0.951056516295154,1.,0.951056516295154,1.,0.951056516295154,1.,0.951056516295154,
1.,0.951056516295154,1.,0.951056516295154,1.,0.951056516295154,1.,0.951056516295154,
1.,0.951056516295154,1.,0.951056516295154,1.,0.951056516295154,1.,0.951056516295154,
1.,0.951056516295154,1.,0.951056516295154,1.,0.951056516295154,1.,0.951056516295154,
1.,0.951056516295154,1.,0.951056516295154,1.,0.951056516295154,1.,0.951056516295154,
1.,0.951056516295154,1.,0.951056516295154,1.,0.951056516295154,1.,0.951056516295154,
1.,0.951056516295154,1.,0.951056516295154,1.,0.951056516295154,1.,0.951056516295154,
1.,0.951056516295154,1.,0.951056516295154,1.,0.951056516295154,1.,0.951056516295154,
1.,0.951056516295154,1.,0.951056516295154,1.,0.951056516295154,1.,0.951056516295154,
1.,0.951056516295154,1.,0.951056516295154,1.,0.951056516295154,1.,0.951056516295154,
1.,0.951056516295154,1.,0.951056516295154,1.,0.951056516295154,1.,0.951056516295154,
1.,0.951056516295154,1.,0.951056516295154,1.,0.951056516295154,1.,0.951056516295154,
1.,0.951056516295154,1.,0.951056516295154,1.,0.951056516295154,1.,0.951056516295154,
1.,0.951056516295154,1.,0.951056516295154,1.,0.951056516295154,1.,0.951056516295154,
1.,0.951056516295154,1.,0.951056516295154,1.,0.951056516295154,1.,0.951056516295154,
1.,0.951056516295154,1.,0.951056516295154,1.,0.951056516295154,1.,0.951056516295154,
1.,0.951056516295154,1.,0.951056516295154,1.,0.951056516295154,1.,0.951056516295154,
1.,0.951056516295154,1.,0.951056516295154,1.,0.951056516295154,1.,0.951056516295154,
1.,0.973808312264696,0.975649140995143)))
REPRESENTATION_ITEM('')
SURFACE()
);
#301=(
BOUNDED_SURFACE()
B_SPLINE_SURFACE(3,2,((#28323,#28324,#28325),(#28326,#28327,#28328),(#28329,
#28330,#28331),(#28332,#28333,#28334),(#28335,#28336,#28337),(#28338,#28339,
#28340),(#28341,#28342,#28343),(#28344,#28345,#28346),(#28347,#28348,#28349),
(#28350,#28351,#28352)),.UNSPECIFIED.,.F.,.F.,.F.)
B_SPLINE_SURFACE_WITH_KNOTS((4,2,2,2,4),(3,3),(0.00398013717080998,0.00543136490531493,
0.00682381476862857,0.00821626463194221,0.00960871449525586),(0.4504813546384,
1.00005877787119),.UNSPECIFIED.)
GEOMETRIC_REPRESENTATION_ITEM()
RATIONAL_B_SPLINE_SURFACE(((0.876526511260875,0.862952378099386,1.00002931931674),
(0.896639296968354,0.885276275149306,1.00002454344832),(0.914408347469022,
0.904998777035469,1.00002032411003),(0.944823095920487,0.938757189375995,
1.00001310199577),(0.957749166091975,0.953104294941835,1.00001003264421),
(0.978422485020086,0.976050347773278,1.00000512367475),(0.986354320920379,
0.984854174882576,1.00000324022583),(0.997174546550185,0.9968639286049,
1.00000067091621),(1.00000968195182,1.00001074634309,0.999999997700978),
(1.,1.,1.)))
REPRESENTATION_ITEM('')
SURFACE()
);
#302=(
BOUNDED_SURFACE()
B_SPLINE_SURFACE(3,2,((#28365,#28366,#28367),(#28368,#28369,#28370),(#28371,
#28372,#28373),(#28374,#28375,#28376),(#28377,#28378,#28379),(#28380,#28381,
#28382),(#28383,#28384,#28385),(#28386,#28387,#28388),(#28389,#28390,#28391),
(#28392,#28393,#28394),(#28395,#28396,#28397),(#28398,#28399,#28400),(#28401,
#28402,#28403),(#28404,#28405,#28406),(#28407,#28408,#28409),(#28410,#28411,
#28412),(#28413,#28414,#28415),(#28416,#28417,#28418),(#28419,#28420,#28421),
(#28422,#28423,#28424),(#28425,#28426,#28427),(#28428,#28429,#28430),(#28431,
#28432,#28433),(#28434,#28435,#28436),(#28437,#28438,#28439),(#28440,#28441,
#28442),(#28443,#28444,#28445),(#28446,#28447,#28448),(#28449,#28450,#28451),
(#28452,#28453,#28454)),.UNSPECIFIED.,.F.,.F.,.F.)
B_SPLINE_SURFACE_WITH_KNOTS((4,2,2,2,2,2,2,2,2,2,2,2,2,2,4),(3,3),(0.,0.0023928943576613,
0.00358934153649195,0.0047857887153226,0.00598223589415325,0.0071786830729839,
0.0095715774306452,0.0101698010200605,0.0107680246094759,0.0119644717883065,
0.0131609189671372,0.0143573661459678,0.0155538133247985,0.0167502605036291,
0.0191431548612904),(0.,1.),.UNSPECIFIED.)
GEOMETRIC_REPRESENTATION_ITEM()
RATIONAL_B_SPLINE_SURFACE(((1.,0.755519678577116,1.),(1.,0.767712634757759,
1.),(1.,0.780608196095567,1.),(1.,0.79934306756545,1.),(1.,0.80552470893265,
1.),(1.,0.817270248347207,1.),(1.,0.822799993283502,1.),(1.,0.832991457849502,
1.),(1.,0.837654127549585,1.),(1.,0.845923910809236,1.),(1.,0.849550572374246,
1.),(1.,0.85828554581335,1.),(1.,0.861359462352663,1.),(1.,0.86139338043001,
1.),(1.,0.861206147953501,1.),(1.,0.860450812266049,1.),(1.,0.859884337138352,
1.),(1.,0.857640585891707,1.),(1.,0.855419731623233,1.),(1.,0.849623257971125,
1.),(1.,0.846014379835457,1.),(1.,0.837715224709792,1.),(1.,0.833033055512742,
1.),(1.,0.822797218586941,1.),(1.,0.817242571682893,1.),(1.,0.805445312247108,
1.),(1.,0.799306345600238,1.),(1.,0.780606551099107,1.),(1.,0.767720440554272,
1.),(1.,0.755519678577116,1.)))
REPRESENTATION_ITEM('')
SURFACE()
);
#303=(
BOUNDED_SURFACE()
B_SPLINE_SURFACE(3,2,((#28549,#28550,#28551),(#28552,#28553,#28554),(#28555,
#28556,#28557),(#28558,#28559,#28560),(#28561,#28562,#28563),(#28564,#28565,
#28566),(#28567,#28568,#28569),(#28570,#28571,#28572),(#28573,#28574,#28575),
(#28576,#28577,#28578)),.UNSPECIFIED.,.F.,.F.,.F.)
B_SPLINE_SURFACE_WITH_KNOTS((4,2,2,2,4),(3,3),(0.00398006295905424,0.00543136490531495,
0.0068238147686286,0.00821626463194225,0.0096087144952559),(-5.88520829470716E-5,
0.549518434171745),.UNSPECIFIED.)
GEOMETRIC_REPRESENTATION_ITEM()
RATIONAL_B_SPLINE_SURFACE(((1.0000293570705,0.862949004176479,0.876523415273787),
(1.00002457487029,0.885274300596315,0.896637470909482),(1.00002034996106,
0.904997931282859,0.914407546500262),(1.00001311853906,0.938757212096139,
0.944823091258541),(1.00001004531197,0.953104312339345,0.957749162522093),
(1.00000513014418,0.976050356658273,0.978422483197019),(1.00000324431711,
0.984854180501291,0.986354319767304),(1.00000067176334,0.996863929768465,
0.997174546311578),(0.999999997698076,1.00001074633898,1.00000968195253),
(1.,1.,1.)))
REPRESENTATION_ITEM('')
SURFACE()
);
#304=(
BOUNDED_SURFACE()
B_SPLINE_SURFACE(3,2,((#28591,#28592,#28593),(#28594,#28595,#28596),(#28597,
#28598,#28599),(#28600,#28601,#28602),(#28603,#28604,#28605),(#28606,#28607,
#28608),(#28609,#28610,#28611),(#28612,#28613,#28614),(#28615,#28616,#28617),
(#28618,#28619,#28620)),.UNSPECIFIED.,.F.,.F.,.F.)
B_SPLINE_SURFACE_WITH_KNOTS((4,2,2,2,4),(3,3),(0.00398013717069273,0.00543136490531495,
0.00682381476862858,0.0082162646319422,0.00960871449525583),(0.450481354362641,
1.00005877787131),.UNSPECIFIED.)
GEOMETRIC_REPRESENTATION_ITEM()
RATIONAL_B_SPLINE_SURFACE(((0.8765265112696,0.862952378025167,1.00002931931679),
(0.896639296976939,0.885276275088599,1.00002454344837),(0.91440834747712,
0.904998776986295,1.00002032411007),(0.944823095926639,0.938757189345328,
1.0000131019958),(0.957749166096613,0.953104294918273,1.00001003264423),
(0.978422485022468,0.97605034776126,1.00000512367476),(0.986354320921773,
0.984854174874851,1.00000324022583),(0.997174546550589,0.996863928603428,
1.00000067091621),(1.00000968195173,1.00001074634299,0.999999997700978),
(1.,1.,1.)))
REPRESENTATION_ITEM('')
SURFACE()
);
#305=(
BOUNDED_SURFACE()
B_SPLINE_SURFACE(3,2,((#28633,#28634,#28635),(#28636,#28637,#28638),(#28639,
#28640,#28641),(#28642,#28643,#28644),(#28645,#28646,#28647),(#28648,#28649,
#28650),(#28651,#28652,#28653),(#28654,#28655,#28656),(#28657,#28658,#28659),
(#28660,#28661,#28662),(#28663,#28664,#28665),(#28666,#28667,#28668),(#28669,
#28670,#28671),(#28672,#28673,#28674),(#28675,#28676,#28677),(#28678,#28679,
#28680),(#28681,#28682,#28683),(#28684,#28685,#28686),(#28687,#28688,#28689),
(#28690,#28691,#28692),(#28693,#28694,#28695),(#28696,#28697,#28698),(#28699,
#28700,#28701),(#28702,#28703,#28704),(#28705,#28706,#28707),(#28708,#28709,
#28710),(#28711,#28712,#28713),(#28714,#28715,#28716),(#28717,#28718,#28719),
(#28720,#28721,#28722)),.UNSPECIFIED.,.F.,.F.,.F.)
B_SPLINE_SURFACE_WITH_KNOTS((4,2,2,2,2,2,2,2,2,2,2,2,2,2,4),(3,3),(0.,0.00239289435766131,
0.00358934153649196,0.00478578871532262,0.00598223589415327,0.00717868307298392,
0.00957157743064523,0.0101698010200606,0.0107680246094759,0.0119644717883065,
0.0131609189671372,0.0143573661459678,0.0155538133247985,0.0167502605036292,
0.0191431548612905),(0.,1.),.UNSPECIFIED.)
GEOMETRIC_REPRESENTATION_ITEM()
RATIONAL_B_SPLINE_SURFACE(((1.,0.755519678577118,1.),(1.,0.767712634757661,
1.),(1.,0.780608196095702,1.),(1.,0.799343067565385,1.),(1.,0.805524708932718,
1.),(1.,0.817270248347141,1.),(1.,0.822799993283503,1.),(1.,0.832991457849504,
1.),(1.,0.837654127549563,1.),(1.,0.845923910809259,1.),(1.,0.849550572374269,
1.),(1.,0.858285545813306,1.),(1.,0.861359462352663,1.),(1.,0.86139338043001,
1.),(1.,0.861206147953501,1.),(1.,0.860450812266049,1.),(1.,0.859884337138363,
1.),(1.,0.857640585891685,1.),(1.,0.8554197316233,1.),(1.,0.849623257971058,
1.),(1.,0.84601437983548,1.),(1.,0.837715224709771,1.),(1.,0.833033055512787,
1.),(1.,0.822797218586897,1.),(1.,0.817242571682917,1.),(1.,0.805445312247087,
1.),(1.,0.799306345600284,1.),(1.,0.780606551099021,1.),(1.,0.767720440554341,
1.),(1.,0.755519678577118,1.)))
REPRESENTATION_ITEM('')
SURFACE()
);
#306=(
BOUNDED_SURFACE()
B_SPLINE_SURFACE(3,2,((#28817,#28818,#28819),(#28820,#28821,#28822),(#28823,
#28824,#28825),(#28826,#28827,#28828),(#28829,#28830,#28831),(#28832,#28833,
#28834),(#28835,#28836,#28837),(#28838,#28839,#28840),(#28841,#28842,#28843),
(#28844,#28845,#28846)),.UNSPECIFIED.,.F.,.F.,.F.)
B_SPLINE_SURFACE_WITH_KNOTS((4,2,2,2,4),(3,3),(0.00398006295938679,0.00543136490531494,
0.00682381476862857,0.0082162646319422,0.00960871449525583),(-5.88520826145246E-5,
0.549518433842917),.UNSPECIFIED.)
GEOMETRIC_REPRESENTATION_ITEM()
RATIONAL_B_SPLINE_SURFACE(((1.00002935707033,0.862949004273862,0.876523415271378),
(1.00002457487015,0.885274300673986,0.896637470903998),(1.00002034996095,
0.904997931343717,0.914407546492603),(1.00001311853899,0.938757212132757,
0.944823091251248),(1.00001004531191,0.953104312367488,0.957749162516602),
(1.00000513014415,0.976050356672542,0.978422483194122),(1.00000324431709,
0.984854180510462,0.986354319765605),(1.00000067176334,0.996863929770251,
0.997174546311125),(0.999999997698075,1.00001074633906,1.00000968195261),
(1.,1.,1.)))
REPRESENTATION_ITEM('')
SURFACE()
);
#307=(
BOUNDED_SURFACE()
B_SPLINE_SURFACE(3,2,((#28859,#28860,#28861),(#28862,#28863,#28864),(#28865,
#28866,#28867),(#28868,#28869,#28870),(#28871,#28872,#28873),(#28874,#28875,
#28876),(#28877,#28878,#28879),(#28880,#28881,#28882),(#28883,#28884,#28885),
(#28886,#28887,#28888),(#28889,#28890,#28891),(#28892,#28893,#28894),(#28895,
#28896,#28897),(#28898,#28899,#28900),(#28901,#28902,#28903),(#28904,#28905,
#28906)),.UNSPECIFIED.,.F.,.F.,.F.)
B_SPLINE_SURFACE_WITH_KNOTS((4,2,2,2,2,2,2,4),(3,3),(-0.000112562685732122,
0.000183317511890047,0.000366635023783252,0.000733270047569662,0.00109990507135607,
0.00146654009514248,0.0021998101427153,0.00293308019028812),(0.,1.00011256268573),
 .UNSPECIFIED.)
GEOMETRIC_REPRESENTATION_ITEM()
RATIONAL_B_SPLINE_SURFACE(((1.,0.888568848431313,1.00002508597939),(1.,
0.914720098615804,1.00001919866948),(1.,0.926614357760784,1.00001652096997),
(1.,0.941497644191807,1.00001317036458),(1.,0.945991617994044,1.00001215865706),
(1.,0.957827766219728,1.00000949403979),(1.,0.963503346961192,1.00000821632257),
(1.,0.973100607067783,1.00000605573583),(1.,0.976922506379337,1.00000519532932),
(1.,0.983418125950154,1.00000373300055),(1.,0.986078267870898,1.00000313413512),
(1.,0.992789809396114,1.00000162319684),(1.,0.995607448637691,1.00000098887476),
(1.,0.99922902552814,1.00000017356591),(1.,0.999994157715377,1.00000000131525),
(1.,1.,1.)))
REPRESENTATION_ITEM('')
SURFACE()
);
#308=(
BOUNDED_SURFACE()
B_SPLINE_SURFACE(3,2,((#28908,#28909,#28910),(#28911,#28912,#28913),(#28914,
#28915,#28916),(#28917,#28918,#28919),(#28920,#28921,#28922),(#28923,#28924,
#28925)),.UNSPECIFIED.,.F.,.F.,.F.)
B_SPLINE_SURFACE_WITH_KNOTS((4,2,4),(3,3),(-2.51534904016637E-17,0.00233940766482981,
0.00467881532965964),(0.,1.),.UNSPECIFIED.)
GEOMETRIC_REPRESENTATION_ITEM()
RATIONAL_B_SPLINE_SURFACE(((1.,0.707106781186545,1.),(1.,0.737898683933714,
1.),(1.,0.772355112026995,1.),(1.,0.844136160947679,1.),(1.,0.88073843286887,
1.),(1.,0.912870929175271,1.)))
REPRESENTATION_ITEM('')
SURFACE()
);
#309=(
BOUNDED_SURFACE()
B_SPLINE_SURFACE(3,2,((#28926,#28927,#28928),(#28929,#28930,#28931),(#28932,
#28933,#28934),(#28935,#28936,#28937),(#28938,#28939,#28940),(#28941,#28942,
#28943),(#28944,#28945,#28946),(#28947,#28948,#28949)),.UNSPECIFIED.,.F.,
 .F.,.F.)
B_SPLINE_SURFACE_WITH_KNOTS((4,2,2,4),(3,3),(-6.98226199080665E-17,0.00233568752491197,
0.00350353128736798,0.004671375049824),(0.,1.),.UNSPECIFIED.)
GEOMETRIC_REPRESENTATION_ITEM()
RATIONAL_B_SPLINE_SURFACE(((1.,0.912870929175276,1.),(1.,0.880766500224452,
1.),(1.,0.84428481138994,1.),(1.,0.7909171071033,1.),(1.,0.773315924547783,
1.),(1.,0.739103003635572,1.),(1.,0.722569869246584,1.),(1.,0.707106781186588,
1.)))
REPRESENTATION_ITEM('')
SURFACE()
);
#310=(
BOUNDED_SURFACE()
B_SPLINE_SURFACE(3,2,((#28951,#28952,#28953),(#28954,#28955,#28956),(#28957,
#28958,#28959),(#28960,#28961,#28962),(#28963,#28964,#28965),(#28966,#28967,
#28968),(#28969,#28970,#28971),(#28972,#28973,#28974),(#28975,#28976,#28977),
(#28978,#28979,#28980),(#28981,#28982,#28983),(#28984,#28985,#28986),(#28987,
#28988,#28989),(#28990,#28991,#28992),(#28993,#28994,#28995),(#28996,#28997,
#28998)),.UNSPECIFIED.,.F.,.F.,.F.)
B_SPLINE_SURFACE_WITH_KNOTS((4,2,2,2,2,2,2,4),(3,3),(-1.60420989719343E-5,
0.000718638734763963,0.00145331956849986,0.00182065998536781,0.00218800040223576,
0.0025553408191037,0.00273901102753768,0.00303146126452106),(0.,1.00010878002855),
 .UNSPECIFIED.)
GEOMETRIC_REPRESENTATION_ITEM()
RATIONAL_B_SPLINE_SURFACE(((1.,1.,1.),(1.,0.999993811318941,1.00000000134641),
(1.,0.999229107803248,1.00000016771535),(1.,0.995637462429539,1.00000094911392),
(1.,0.992845445901653,1.0000015565452),(1.,0.986217024917209,1.00000299862485),
(1.,0.983595353986027,1.00000356899572),(1.,0.977148768484335,1.00000497151523),
(1.,0.973342745657784,1.00000579955378),(1.,0.963689034415866,1.00000789981575),
(1.,0.957941368212052,1.00000915027833),(1.,0.946018892185112,1.0000117441329),
(1.,0.941495863696682,1.00001272816323),(1.,0.92668492389742,1.00001595043214),
(1.,0.914960830141336,1.00001850112665),(1.,0.889823099708682,1.00002397009272)))
REPRESENTATION_ITEM('')
SURFACE()
);
#311=(
BOUNDED_SURFACE()
B_SPLINE_SURFACE(3,2,((#28999,#29000,#29001),(#29002,#29003,#29004),(#29005,
#29006,#29007),(#29008,#29009,#29010),(#29011,#29012,#29013),(#29014,#29015,
#29016),(#29017,#29018,#29019),(#29020,#29021,#29022),(#29023,#29024,#29025),
(#29026,#29027,#29028),(#29029,#29030,#29031),(#29032,#29033,#29034),(#29035,
#29036,#29037),(#29038,#29039,#29040),(#29041,#29042,#29043),(#29044,#29045,
#29046)),.UNSPECIFIED.,.F.,.F.,.F.)
B_SPLINE_SURFACE_WITH_KNOTS((4,2,2,2,2,2,2,4),(3,3),(-1.60420989715478E-5,
0.000723179017757225,0.001462400134486,0.00183201069285038,0.00220162125121477,
0.00257123180957916,0.00275603708876135,0.00304759539405443),(0.,1.00010675302611),
 .UNSPECIFIED.)
GEOMETRIC_REPRESENTATION_ITEM()
RATIONAL_B_SPLINE_SURFACE(((1.,1.,1.),(1.,0.999993484045624,1.0000000013912),
(1.,0.999229603748512,1.00000016448426),(1.,0.995614556488104,1.00000093631873),
(1.,0.992787523332635,1.00000153990742),(1.,0.986117874326191,1.00000296391785),
(1.,0.983484316794167,1.00000352619832),(1.,0.977034241545352,1.00000490332842),
(1.,0.973235033264553,1.00000571448239),(1.,0.963662174424421,1.00000775834569),
(1.,0.957994029080871,1.00000896852902),(1.,0.946081971657189,1.00001151182537),
(1.,0.941528775727103,1.00001248396026),(1.,0.92674259996446,1.00001564089828),
(1.,0.915116673686062,1.0000181231039),(1.,0.890638328972987,1.00002334937864)))
REPRESENTATION_ITEM('')
SURFACE()
);
#312=(
BOUNDED_SURFACE()
B_SPLINE_SURFACE(3,2,((#29048,#29049,#29050),(#29051,#29052,#29053),(#29054,
#29055,#29056),(#29057,#29058,#29059),(#29060,#29061,#29062),(#29063,#29064,
#29065),(#29066,#29067,#29068),(#29069,#29070,#29071)),.UNSPECIFIED.,.F.,
 .F.,.F.)
B_SPLINE_SURFACE_WITH_KNOTS((4,2,2,4),(3,3),(9.30245463992563E-17,0.00233568752491339,
0.00350353128737004,0.00467137504982669),(0.,1.),.UNSPECIFIED.)
GEOMETRIC_REPRESENTATION_ITEM()
RATIONAL_B_SPLINE_SURFACE(((1.,0.912870929175271,1.),(1.,0.880766500224456,
1.),(1.,0.84428481138985,1.),(1.,0.790917107103246,1.),(1.,0.773315924547701,
1.),(1.,0.739103003635471,1.),(1.,0.722569869246403,1.),(1.,0.707106781186576,
1.)))
REPRESENTATION_ITEM('')
SURFACE()
);
#313=(
BOUNDED_SURFACE()
B_SPLINE_SURFACE(3,2,((#29072,#29073,#29074),(#29075,#29076,#29077),(#29078,
#29079,#29080),(#29081,#29082,#29083),(#29084,#29085,#29086),(#29087,#29088,
#29089)),.UNSPECIFIED.,.F.,.F.,.F.)
B_SPLINE_SURFACE_WITH_KNOTS((4,2,4),(3,3),(4.33680868994202E-17,0.00233940766482989,
0.00467881532965973),(0.,1.),.UNSPECIFIED.)
GEOMETRIC_REPRESENTATION_ITEM()
RATIONAL_B_SPLINE_SURFACE(((1.,0.707106781186544,1.),(1.,0.737898683933686,
1.),(1.,0.772355112027042,1.),(1.,0.844136160947639,1.),(1.,0.880738432868901,
1.),(1.,0.912870929175275,1.)))
REPRESENTATION_ITEM('')
SURFACE()
);
#314=(
BOUNDED_SURFACE()
B_SPLINE_SURFACE(3,2,((#29091,#29092,#29093),(#29094,#29095,#29096),(#29097,
#29098,#29099),(#29100,#29101,#29102),(#29103,#29104,#29105),(#29106,#29107,
#29108),(#29109,#29110,#29111),(#29112,#29113,#29114),(#29115,#29116,#29117),
(#29118,#29119,#29120),(#29121,#29122,#29123),(#29124,#29125,#29126),(#29127,
#29128,#29129),(#29130,#29131,#29132),(#29133,#29134,#29135),(#29136,#29137,
#29138)),.UNSPECIFIED.,.F.,.F.,.F.)
B_SPLINE_SURFACE_WITH_KNOTS((4,2,2,2,2,2,2,4),(3,3),(-0.000112562684352504,
0.000183317511890177,0.000366635023783385,0.000733270047569803,0.00109990507135622,
0.00146654009514264,0.00219981014271547,0.00293308019028831),(0.,1.00011256268435),
 .UNSPECIFIED.)
GEOMETRIC_REPRESENTATION_ITEM()
RATIONAL_B_SPLINE_SURFACE(((1.,0.888568848797213,1.000025085979),(1.,0.914720098726859,
1.00001919866922),(1.,0.926614357803736,1.00001652096976),(1.,0.941497644191894,
1.00001317036442),(1.,0.945991617994114,1.00001215865691),(1.,0.957827766219802,
1.00000949403968),(1.,0.963503346961249,1.00000821632247),(1.,0.973100607067813,
1.00000605573575),(1.,0.976922506379361,1.00000519532926),(1.,0.983418125950182,
1.00000373300051),(1.,0.986078267870914,1.00000313413508),(1.,0.992789809396121,
1.00000162319682),(1.,0.995607448637693,1.00000098887474),(1.,0.999229025528137,
1.00000017356591),(1.,0.999994157715368,1.00000000131525),(1.,1.,1.)))
REPRESENTATION_ITEM('')
SURFACE()
);
#315=(
BOUNDED_SURFACE()
B_SPLINE_SURFACE(1,2,((#30077,#30078,#30079,#30080,#30081,#30082,#30083,
#30084,#30085,#30086,#30087,#30088,#30089,#30090,#30091,#30092,#30093,#30094,
#30095,#30096,#30097,#30098,#30099,#30100,#30101,#30102,#30103,#30104,#30105,
#30106,#30107,#30108,#30109,#30110,#30111,#30112,#30113,#30114,#30115,#30116,
#30117,#30118,#30119,#30120,#30121,#30122,#30123,#30124,#30125,#30126,#30127,
#30128,#30129,#30130,#30131,#30132,#30133,#30134,#30135,#30136,#30137,#30138,
#30139,#30140,#30141,#30142,#30143,#30144,#30145,#30146,#30147,#30148,#30149,
#30150,#30151,#30152,#30153,#30154,#30155,#30156,#30157,#30158,#30159,#30160,
#30161,#30162,#30163,#30164,#30165,#30166,#30167,#30168,#30169,#30170,#30171,
#30172,#30173,#30174,#30175,#30176,#30177,#30178,#30179,#30180,#30181,#30182,
#30183,#30184,#30185,#30186,#30187,#30188,#30189,#30190,#30191,#30192,#30193,
#30194,#30195,#30196,#30197,#30198,#30199,#30200,#30201,#30202,#30203,#30204,
#30205,#30206,#30207,#30208,#30209,#30210,#30211,#30212,#30213),(#30214,
#30215,#30216,#30217,#30218,#30219,#30220,#30221,#30222,#30223,#30224,#30225,
#30226,#30227,#30228,#30229,#30230,#30231,#30232,#30233,#30234,#30235,#30236,
#30237,#30238,#30239,#30240,#30241,#30242,#30243,#30244,#30245,#30246,#30247,
#30248,#30249,#30250,#30251,#30252,#30253,#30254,#30255,#30256,#30257,#30258,
#30259,#30260,#30261,#30262,#30263,#30264,#30265,#30266,#30267,#30268,#30269,
#30270,#30271,#30272,#30273,#30274,#30275,#30276,#30277,#30278,#30279,#30280,
#30281,#30282,#30283,#30284,#30285,#30286,#30287,#30288,#30289,#30290,#30291,
#30292,#30293,#30294,#30295,#30296,#30297,#30298,#30299,#30300,#30301,#30302,
#30303,#30304,#30305,#30306,#30307,#30308,#30309,#30310,#30311,#30312,#30313,
#30314,#30315,#30316,#30317,#30318,#30319,#30320,#30321,#30322,#30323,#30324,
#30325,#30326,#30327,#30328,#30329,#30330,#30331,#30332,#30333,#30334,#30335,
#30336,#30337,#30338,#30339,#30340,#30341,#30342,#30343,#30344,#30345,#30346,
#30347,#30348,#30349,#30350)),.UNSPECIFIED.,.F.,.F.,.F.)
B_SPLINE_SURFACE_WITH_KNOTS((2,2),(3,2,2,2,2,2,2,2,2,2,2,2,2,2,2,2,2,2,
2,2,2,2,2,2,2,2,2,2,2,2,2,2,2,2,2,2,2,2,2,2,2,2,2,2,2,2,2,2,2,2,2,2,2,2,
2,2,2,2,2,2,2,2,2,2,2,2,2,2,3),(0.,1.),(0.,0.0142857142857143,0.0285714285714286,
0.0428571428571429,0.0571428571428571,0.0714285714285714,0.0857142857142857,
0.1,0.114285714285714,0.128571428571429,0.142857142857143,0.157142857142857,
0.171428571428571,0.185714285714286,0.2,0.214285714285714,0.228571428571429,
0.242857142857143,0.257142857142857,0.271428571428571,0.285714285714286,
0.3,0.314285714285714,0.328571428571429,0.342857142857143,0.357142857142857,
0.371428571428571,0.385714285714286,0.4,0.414285714285714,0.428571428571429,
0.442857142857143,0.457142857142857,0.471428571428571,0.485714285714286,
0.5,0.514285714285714,0.528571428571429,0.542857142857143,0.557142857142857,
0.571428571428571,0.585714285714286,0.6,0.614285714285714,0.628571428571429,
0.642857142857143,0.657142857142857,0.671428571428571,0.685714285714286,
0.7,0.714285714285714,0.728571428571429,0.742857142857143,0.757142857142857,
0.771428571428571,0.785714285714286,0.8,0.814285714285714,0.828571428571429,
0.842857142857143,0.857142857142857,0.871428571428571,0.885714285714286,
0.9,0.914285714285714,0.928571428571429,0.942857142857143,0.957142857142857,
0.961773175750461),.UNSPECIFIED.)
GEOMETRIC_REPRESENTATION_ITEM()
RATIONAL_B_SPLINE_SURFACE(((1.,0.951056516295154,1.,0.951056516295154,1.,
0.951056516295154,1.,0.951056516295154,1.,0.951056516295154,1.,0.951056516295154,
1.,0.951056516295154,1.,0.951056516295154,1.,0.951056516295154,1.,0.951056516295154,
1.,0.951056516295154,1.,0.951056516295154,1.,0.951056516295154,1.,0.951056516295154,
1.,0.951056516295154,1.,0.951056516295154,1.,0.951056516295154,1.,0.951056516295154,
1.,0.951056516295154,1.,0.951056516295154,1.,0.951056516295154,1.,0.951056516295154,
1.,0.951056516295154,1.,0.951056516295154,1.,0.951056516295154,1.,0.951056516295154,
1.,0.951056516295154,1.,0.951056516295154,1.,0.951056516295154,1.,0.951056516295154,
1.,0.951056516295154,1.,0.951056516295154,1.,0.951056516295154,1.,0.951056516295154,
1.,0.951056516295154,1.,0.951056516295154,1.,0.951056516295154,1.,0.951056516295154,
1.,0.951056516295154,1.,0.951056516295154,1.,0.951056516295154,1.,0.951056516295154,
1.,0.951056516295154,1.,0.951056516295154,1.,0.951056516295154,1.,0.951056516295154,
1.,0.951056516295154,1.,0.951056516295154,1.,0.951056516295154,1.,0.951056516295154,
1.,0.951056516295154,1.,0.951056516295154,1.,0.951056516295154,1.,0.951056516295154,
1.,0.951056516295154,1.,0.951056516295154,1.,0.951056516295154,1.,0.951056516295154,
1.,0.951056516295154,1.,0.951056516295154,1.,0.951056516295154,1.,0.951056516295154,
1.,0.951056516295154,1.,0.951056516295154,1.,0.951056516295154,1.,0.951056516295154,
1.,0.951056516295154,1.,0.984136325367634,0.978556192232199),(1.,0.951056516295154,
1.,0.951056516295154,1.,0.951056516295154,1.,0.951056516295154,1.,0.951056516295154,
1.,0.951056516295154,1.,0.951056516295154,1.,0.951056516295154,1.,0.951056516295154,
1.,0.951056516295154,1.,0.951056516295154,1.,0.951056516295154,1.,0.951056516295154,
1.,0.951056516295154,1.,0.951056516295154,1.,0.951056516295154,1.,0.951056516295154,
1.,0.951056516295154,1.,0.951056516295154,1.,0.951056516295154,1.,0.951056516295154,
1.,0.951056516295154,1.,0.951056516295154,1.,0.951056516295154,1.,0.951056516295154,
1.,0.951056516295154,1.,0.951056516295154,1.,0.951056516295154,1.,0.951056516295154,
1.,0.951056516295154,1.,0.951056516295154,1.,0.951056516295154,1.,0.951056516295154,
1.,0.951056516295154,1.,0.951056516295154,1.,0.951056516295154,1.,0.951056516295154,
1.,0.951056516295154,1.,0.951056516295154,1.,0.951056516295154,1.,0.951056516295154,
1.,0.951056516295154,1.,0.951056516295154,1.,0.951056516295154,1.,0.951056516295154,
1.,0.951056516295154,1.,0.951056516295154,1.,0.951056516295154,1.,0.951056516295154,
1.,0.951056516295154,1.,0.951056516295154,1.,0.951056516295154,1.,0.951056516295154,
1.,0.951056516295154,1.,0.951056516295154,1.,0.951056516295154,1.,0.951056516295154,
1.,0.951056516295154,1.,0.951056516295154,1.,0.951056516295154,1.,0.951056516295154,
1.,0.951056516295154,1.,0.951056516295154,1.,0.951056516295154,1.,0.951056516295154,
1.,0.951056516295154,1.,0.951056516295154,1.,0.984136325367634,0.978556192232199)))
REPRESENTATION_ITEM('')
SURFACE()
);
#316=(
BOUNDED_SURFACE()
B_SPLINE_SURFACE(1,2,((#30394,#30395,#30396,#30397,#30398,#30399,#30400,
#30401,#30402,#30403,#30404,#30405,#30406,#30407,#30408,#30409,#30410,#30411,
#30412,#30413,#30414,#30415,#30416,#30417,#30418,#30419,#30420,#30421,#30422,
#30423,#30424,#30425,#30426,#30427,#30428,#30429,#30430,#30431,#30432,#30433,
#30434,#30435,#30436,#30437,#30438,#30439,#30440,#30441,#30442,#30443,#30444,
#30445,#30446,#30447,#30448,#30449,#30450,#30451,#30452,#30453,#30454,#30455,
#30456,#30457,#30458,#30459,#30460,#30461,#30462,#30463,#30464,#30465,#30466,
#30467,#30468,#30469,#30470,#30471,#30472,#30473,#30474,#30475,#30476,#30477,
#30478,#30479,#30480,#30481,#30482,#30483,#30484,#30485,#30486,#30487,#30488,
#30489,#30490,#30491,#30492,#30493,#30494,#30495,#30496,#30497,#30498,#30499,
#30500,#30501,#30502,#30503,#30504,#30505,#30506,#30507,#30508,#30509,#30510,
#30511,#30512,#30513,#30514,#30515,#30516,#30517,#30518,#30519,#30520,#30521,
#30522,#30523,#30524,#30525,#30526,#30527,#30528,#30529,#30530),(#30531,
#30532,#30533,#30534,#30535,#30536,#30537,#30538,#30539,#30540,#30541,#30542,
#30543,#30544,#30545,#30546,#30547,#30548,#30549,#30550,#30551,#30552,#30553,
#30554,#30555,#30556,#30557,#30558,#30559,#30560,#30561,#30562,#30563,#30564,
#30565,#30566,#30567,#30568,#30569,#30570,#30571,#30572,#30573,#30574,#30575,
#30576,#30577,#30578,#30579,#30580,#30581,#30582,#30583,#30584,#30585,#30586,
#30587,#30588,#30589,#30590,#30591,#30592,#30593,#30594,#30595,#30596,#30597,
#30598,#30599,#30600,#30601,#30602,#30603,#30604,#30605,#30606,#30607,#30608,
#30609,#30610,#30611,#30612,#30613,#30614,#30615,#30616,#30617,#30618,#30619,
#30620,#30621,#30622,#30623,#30624,#30625,#30626,#30627,#30628,#30629,#30630,
#30631,#30632,#30633,#30634,#30635,#30636,#30637,#30638,#30639,#30640,#30641,
#30642,#30643,#30644,#30645,#30646,#30647,#30648,#30649,#30650,#30651,#30652,
#30653,#30654,#30655,#30656,#30657,#30658,#30659,#30660,#30661,#30662,#30663,
#30664,#30665,#30666,#30667)),.UNSPECIFIED.,.F.,.F.,.F.)
B_SPLINE_SURFACE_WITH_KNOTS((2,2),(3,2,2,2,2,2,2,2,2,2,2,2,2,2,2,2,2,2,
2,2,2,2,2,2,2,2,2,2,2,2,2,2,2,2,2,2,2,2,2,2,2,2,2,2,2,2,2,2,2,2,2,2,2,2,
2,2,2,2,2,2,2,2,2,2,2,2,2,2,3),(0.,1.),(0.,0.0142857142857143,0.0285714285714286,
0.0428571428571429,0.0571428571428571,0.0714285714285714,0.0857142857142857,
0.1,0.114285714285714,0.128571428571429,0.142857142857143,0.157142857142857,
0.171428571428571,0.185714285714286,0.2,0.214285714285714,0.228571428571429,
0.242857142857143,0.257142857142857,0.271428571428571,0.285714285714286,
0.3,0.314285714285714,0.328571428571429,0.342857142857143,0.357142857142857,
0.371428571428571,0.385714285714286,0.4,0.414285714285714,0.428571428571429,
0.442857142857143,0.457142857142857,0.471428571428571,0.485714285714286,
0.5,0.514285714285714,0.528571428571429,0.542857142857143,0.557142857142857,
0.571428571428571,0.585714285714286,0.6,0.614285714285714,0.628571428571429,
0.642857142857143,0.657142857142857,0.671428571428571,0.685714285714286,
0.7,0.714285714285714,0.728571428571429,0.742857142857143,0.757142857142857,
0.771428571428571,0.785714285714286,0.8,0.814285714285714,0.828571428571429,
0.842857142857143,0.857142857142857,0.871428571428571,0.885714285714286,
0.9,0.914285714285714,0.928571428571429,0.942857142857143,0.957142857142857,
0.961773131622773),.UNSPECIFIED.)
GEOMETRIC_REPRESENTATION_ITEM()
RATIONAL_B_SPLINE_SURFACE(((1.,0.951056516295154,1.,0.951056516295154,1.,
0.951056516295154,1.,0.951056516295154,1.,0.951056516295154,1.,0.951056516295154,
1.,0.951056516295154,1.,0.951056516295154,1.,0.951056516295154,1.,0.951056516295154,
1.,0.951056516295154,1.,0.951056516295154,1.,0.951056516295154,1.,0.951056516295154,
1.,0.951056516295154,1.,0.951056516295154,1.,0.951056516295154,1.,0.951056516295154,
1.,0.951056516295154,1.,0.951056516295154,1.,0.951056516295154,1.,0.951056516295154,
1.,0.951056516295154,1.,0.951056516295154,1.,0.951056516295154,1.,0.951056516295154,
1.,0.951056516295154,1.,0.951056516295154,1.,0.951056516295154,1.,0.951056516295154,
1.,0.951056516295154,1.,0.951056516295154,1.,0.951056516295154,1.,0.951056516295154,
1.,0.951056516295154,1.,0.951056516295154,1.,0.951056516295154,1.,0.951056516295154,
1.,0.951056516295154,1.,0.951056516295154,1.,0.951056516295154,1.,0.951056516295154,
1.,0.951056516295154,1.,0.951056516295154,1.,0.951056516295154,1.,0.951056516295154,
1.,0.951056516295154,1.,0.951056516295154,1.,0.951056516295154,1.,0.951056516295154,
1.,0.951056516295154,1.,0.951056516295154,1.,0.951056516295154,1.,0.951056516295154,
1.,0.951056516295154,1.,0.951056516295154,1.,0.951056516295154,1.,0.951056516295154,
1.,0.951056516295154,1.,0.951056516295154,1.,0.951056516295154,1.,0.951056516295154,
1.,0.951056516295154,1.,0.951056516295154,1.,0.951056516295154,1.,0.951056516295154,
1.,0.951056516295154,1.,0.98413647655103,0.978556298592283),(1.,0.951056516295154,
1.,0.951056516295154,1.,0.951056516295154,1.,0.951056516295154,1.,0.951056516295154,
1.,0.951056516295154,1.,0.951056516295154,1.,0.951056516295154,1.,0.951056516295154,
1.,0.951056516295154,1.,0.951056516295154,1.,0.951056516295154,1.,0.951056516295154,
1.,0.951056516295154,1.,0.951056516295154,1.,0.951056516295154,1.,0.951056516295154,
1.,0.951056516295154,1.,0.951056516295154,1.,0.951056516295154,1.,0.951056516295154,
1.,0.951056516295154,1.,0.951056516295154,1.,0.951056516295154,1.,0.951056516295154,
1.,0.951056516295154,1.,0.951056516295154,1.,0.951056516295154,1.,0.951056516295154,
1.,0.951056516295154,1.,0.951056516295154,1.,0.951056516295154,1.,0.951056516295154,
1.,0.951056516295154,1.,0.951056516295154,1.,0.951056516295154,1.,0.951056516295154,
1.,0.951056516295154,1.,0.951056516295154,1.,0.951056516295154,1.,0.951056516295154,
1.,0.951056516295154,1.,0.951056516295154,1.,0.951056516295154,1.,0.951056516295154,
1.,0.951056516295154,1.,0.951056516295154,1.,0.951056516295154,1.,0.951056516295154,
1.,0.951056516295154,1.,0.951056516295154,1.,0.951056516295154,1.,0.951056516295154,
1.,0.951056516295154,1.,0.951056516295154,1.,0.951056516295154,1.,0.951056516295154,
1.,0.951056516295154,1.,0.951056516295154,1.,0.951056516295154,1.,0.951056516295154,
1.,0.951056516295154,1.,0.951056516295154,1.,0.951056516295154,1.,0.951056516295154,
1.,0.951056516295154,1.,0.951056516295154,1.,0.98413647655103,0.978556298592283)))
REPRESENTATION_ITEM('')
SURFACE()
);
#317=B_SPLINE_CURVE_WITH_KNOTS('',3,(#24065,#24066,#24067,#24068,#24069,
#24070,#24071,#24072,#24073,#24074,#24075,#24076,#24077,#24078,#24079,#24080,
#24081,#24082,#24083,#24084,#24085,#24086,#24087,#24088,#24089,#24090,#24091,
#24092,#24093,#24094,#24095,#24096,#24097,#24098,#24099,#24100),
 .UNSPECIFIED.,.F.,.F.,(4,2,2,2,2,2,2,2,2,2,2,2,2,2,2,2,2,4),(-7.02983716919818,
-6.91061727983595,-6.60184957613577,-6.29209349508421,-5.97672564685978,
-5.6693427861326,-5.35705323733312,-5.04620132033749,-4.73820324576839,
-4.4231606033521,-4.11494256505677,-3.80457129106106,-3.49054974125412,
-3.18321904871051,-2.87024417000407,-2.56027854485072,-2.25179476733888,
-2.02069964322786),.UNSPECIFIED.);
#318=B_SPLINE_CURVE_WITH_KNOTS('',3,(#24104,#24105,#24106,#24107,#24108,
#24109,#24110,#24111,#24112,#24113,#24114,#24115,#24116,#24117,#24118,#24119,
#24120,#24121,#24122,#24123,#24124,#24125,#24126,#24127,#24128,#24129,#24130,
#24131,#24132,#24133,#24134,#24135,#24136,#24137,#24138,#24139,#24140,#24141,
#24142,#24143,#24144,#24145,#24146,#24147,#24148,#24149),.UNSPECIFIED.,
 .F.,.F.,(4,3,3,3,3,3,3,3,3,3,3,3,3,3,3,4),(-1.78276958404949E-5,0.00048760205222048,
0.000990696883911432,0.0011620783262953,0.00159313838411329,0.00201847260827172,
0.0023419843484311,0.00264615772116661,0.0029489264191348,0.0032509318938781,
0.0035218903705669,0.00402412376628078,0.0041118433816348,0.00435917421442693,
0.00460747003987267,0.00470179639270271),.UNSPECIFIED.);
#319=B_SPLINE_CURVE_WITH_KNOTS('',3,(#24151,#24152,#24153,#24154,#24155,
#24156,#24157,#24158,#24159,#24160,#24161,#24162,#24163,#24164,#24165,#24166,
#24167,#24168,#24169,#24170,#24171,#24172,#24173,#24174,#24175,#24176,#24177,
#24178,#24179,#24180,#24181,#24182,#24183,#24184,#24185,#24186,#24187,#24188,
#24189,#24190,#24191,#24192,#24193,#24194,#24195,#24196,#24197,#24198,#24199,
#24200,#24201,#24202,#24203,#24204,#24205,#24206,#24207,#24208,#24209,#24210,
#24211,#24212,#24213,#24214,#24215,#24216,#24217,#24218,#24219,#24220,#24221,
#24222,#24223,#24224,#24225,#24226,#24227,#24228,#24229,#24230,#24231,#24232,
#24233,#24234,#24235,#24236,#24237,#24238,#24239,#24240,#24241,#24242,#24243,
#24244,#24245,#24246,#24247,#24248,#24249,#24250,#24251,#24252,#24253,#24254,
#24255,#24256,#24257,#24258,#24259,#24260,#24261,#24262,#24263,#24264,#24265),
 .UNSPECIFIED.,.F.,.F.,(4,3,3,3,3,3,3,3,3,3,3,3,3,3,3,3,3,3,3,3,3,3,3,3,
3,3,3,3,3,3,3,3,3,3,3,3,3,3,4),(0.,0.000835280056435426,0.00169563992176735,
0.00202900517965703,0.00203670118809256,0.00273967946803035,0.00304350776948554,
0.00305586812971479,0.00382326558602126,0.00405801035931406,0.00407363242773161,
0.00488802506566889,0.00507251294914258,0.00508876089012826,0.00571265222895443,
0.0060870155389711,0.00610043813452581,0.00739805770417624,0.00811602071862814,
0.00811729674236745,0.00862041865727346,0.00912389078901127,0.00913052330845666,
0.0101329818752895,0.0101450258982852,0.0107937367146334,0.0111445911494065,
0.0111595284881137,0.0119661634642224,0.0121594862552067,0.0121740310779422,
0.0129702064619354,0.0131770532806838,0.0139835466547703,0.0141959022300147,
0.0142030362575992,0.0150627300415056,0.0158961801336698,0.0162320414372563),
 .UNSPECIFIED.);
#320=B_SPLINE_CURVE_WITH_KNOTS('',3,(#24267,#24268,#24269,#24270,#24271,
#24272,#24273,#24274,#24275,#24276,#24277,#24278,#24279,#24280,#24281,#24282,
#24283,#24284,#24285,#24286,#24287,#24288,#24289,#24290,#24291,#24292,#24293,
#24294,#24295,#24296,#24297,#24298,#24299,#24300,#24301,#24302,#24303,#24304,
#24305,#24306,#24307,#24308,#24309,#24310,#24311,#24312,#24313,#24314,#24315,
#24316,#24317,#24318),.UNSPECIFIED.,.F.,.F.,(4,3,3,3,3,3,3,3,3,3,3,3,3,
3,3,3,3,4),(0.,0.000250783426701624,0.000500478773643964,0.000595498928445555,
0.0011024723631392,0.00119099785689111,0.00149585681270147,0.00180098314939396,
0.00210806480762694,0.00238199571378222,0.00281024881469782,0.00324458797215041,
0.00357299357067334,0.00391657307822326,0.00416849249911889,0.00443812719701021,
0.0047084871246697,0.00476399142756445),.UNSPECIFIED.);
#321=B_SPLINE_CURVE_WITH_KNOTS('',3,(#24320,#24321,#24322,#24323,#24324,
#24325,#24326,#24327,#24328,#24329,#24330,#24331,#24332,#24333,#24334,#24335,
#24336,#24337,#24338,#24339,#24340,#24341,#24342,#24343,#24344,#24345,#24346,
#24347,#24348,#24349,#24350,#24351,#24352,#24353,#24354,#24355,#24356,#24357,
#24358,#24359,#24360,#24361,#24362,#24363,#24364,#24365),.UNSPECIFIED.,
 .F.,.F.,(4,3,3,3,3,3,3,3,3,3,3,3,3,3,3,4),(-1.78276958405635E-5,0.000487602051909098,
0.000990696883295357,0.00116207832629524,0.00159313838411058,0.00201847260826763,
0.00234198434843103,0.0026461577211663,0.0029489264191348,0.00325093189387818,
0.00352189037056683,0.00402412376627937,0.00411184338163473,0.00435917421442732,
0.00460747003987296,0.00470179639270263),.UNSPECIFIED.);
#322=B_SPLINE_CURVE_WITH_KNOTS('',3,(#24367,#24368,#24369,#24370,#24371,
#24372,#24373,#24374,#24375,#24376,#24377,#24378,#24379,#24380,#24381,#24382,
#24383,#24384,#24385,#24386,#24387,#24388,#24389,#24390,#24391,#24392,#24393,
#24394,#24395,#24396,#24397,#24398,#24399,#24400,#24401,#24402,#24403,#24404,
#24405,#24406,#24407,#24408,#24409,#24410,#24411,#24412,#24413,#24414,#24415,
#24416,#24417,#24418,#24419,#24420,#24421,#24422,#24423,#24424,#24425,#24426,
#24427,#24428,#24429,#24430,#24431,#24432,#24433,#24434,#24435,#24436,#24437,
#24438,#24439,#24440,#24441,#24442,#24443,#24444,#24445,#24446,#24447,#24448,
#24449,#24450,#24451,#24452,#24453,#24454,#24455,#24456,#24457,#24458,#24459,
#24460,#24461,#24462,#24463,#24464,#24465,#24466,#24467,#24468,#24469,#24470,
#24471,#24472,#24473,#24474,#24475,#24476,#24477,#24478,#24479,#24480,#24481),
 .UNSPECIFIED.,.F.,.F.,(4,3,3,3,3,3,3,3,3,3,3,3,3,3,3,3,3,3,3,3,3,3,3,3,
3,3,3,3,3,3,3,3,3,3,3,3,3,3,4),(0.,0.000835280057182376,0.00169563992374365,
0.00202900517965707,0.00203670118809262,0.00273967946780872,0.0030435077694856,
0.00305586812971486,0.00382326558623257,0.00405801035931413,0.00407363242773168,
0.00488802506543847,0.00507251294914266,0.00508876089012833,0.00571265222913317,
0.0060870155389712,0.00610043813452591,0.00739805770647065,0.00811602071862826,
0.00811729674236754,0.00862041865727386,0.00912389078901138,0.00913052330845679,
0.0101329818752897,0.0101450258982853,0.0107937367140956,0.0111445911494066,
0.0111595284881138,0.0119661634632636,0.0121594862552069,0.0121740310779424,
0.0129702064615506,0.0131770532806835,0.0139835466544668,0.0141959022300149,
0.0142030362575994,0.015062730039064,0.0158961801294878,0.0162320414372565),
 .UNSPECIFIED.);
#323=B_SPLINE_CURVE_WITH_KNOTS('',3,(#24482,#24483,#24484,#24485,#24486,
#24487,#24488,#24489,#24490,#24491,#24492,#24493,#24494,#24495,#24496,#24497,
#24498,#24499,#24500,#24501,#24502,#24503,#24504,#24505,#24506,#24507,#24508,
#24509,#24510,#24511,#24512,#24513,#24514,#24515,#24516,#24517,#24518,#24519,
#24520,#24521,#24522,#24523,#24524,#24525,#24526,#24527,#24528,#24529,#24530,
#24531,#24532,#24533),.UNSPECIFIED.,.F.,.F.,(4,3,3,3,3,3,3,3,3,3,3,3,3,
3,3,3,3,4),(0.,0.000250783426701639,0.000500478773643702,0.00059549892844555,
0.00110247236313969,0.0011909978568911,0.00149585681270176,0.00180098314939464,
0.00210806480762769,0.0023819957137822,0.00281024881469934,0.00324458797215156,
0.0035729935706733,0.00391657307822337,0.00416849249911885,0.00443812719701222,
0.00470848712467381,0.00476399142756435),.UNSPECIFIED.);
#324=B_SPLINE_CURVE_WITH_KNOTS('',3,(#24535,#24536,#24537,#24538,#24539,
#24540,#24541,#24542,#24543,#24544,#24545,#24546,#24547,#24548,#24549,#24550,
#24551,#24552),.UNSPECIFIED.,.F.,.F.,(4,2,2,2,2,2,2,2,4),(-2.02069964322786,
-1.93602870456447,-1.62817717542802,-1.31711717061402,-1.00426032153936,
-0.696786756318718,-0.383063120605535,-0.192742107424168,-1.68481669504672E-7),
 .UNSPECIFIED.);
#325=B_SPLINE_CURVE_WITH_KNOTS('',3,(#24555,#24556,#24557,#24558,#24559,
#24560,#24561,#24562,#24563,#24564,#24565,#24566,#24567,#24568,#24569,#24570,
#24571,#24572,#24573,#24574,#24575,#24576,#24577,#24578,#24579,#24580,#24581,
#24582),.UNSPECIFIED.,.F.,.F.,(4,2,2,2,2,2,2,2,2,2,2,2,2,4),(-102.474089688378,
-102.46654374275,-102.459658842978,-102.445888796445,-102.418354743121,
-102.363366857814,-102.25415351107,-102.036501710124,-101.720905207923,
-101.412622763323,-101.103211103582,-100.790411499237,-100.483417818375,
-100.455361666765),.UNSPECIFIED.);
#326=B_SPLINE_CURVE_WITH_KNOTS('',3,(#24587,#24588,#24589,#24590,#24591,
#24592,#24593,#24594,#24595,#24596,#24597,#24598,#24599,#24600,#24601,#24602,
#24603,#24604,#24605,#24606,#24607,#24608,#24609,#24610,#24611,#24612,#24613,
#24614,#24615,#24616,#24617,#24618,#24619,#24620,#24621,#24622),
 .UNSPECIFIED.,.F.,.F.,(4,2,2,2,2,2,2,2,2,2,2,2,2,2,2,2,2,4),(-12.038757850411,
-11.8853163131962,-11.5753600418793,-11.2669746154469,-10.9513198822466,
-10.6435111532232,-10.3325590764039,-10.0196946327693,-9.71229683067363,
-9.39868523199586,-9.08943048477653,-8.78038464839336,-8.46395120910075,
-8.15632710992796,-7.8446364669664,-7.53273261566686,-7.22501792738819,
-7.02983716919818),.UNSPECIFIED.);
#327=B_SPLINE_CURVE_WITH_KNOTS('',3,(#24623,#24624,#24625,#24626,#24627,
#24628,#24629,#24630,#24631,#24632,#24633,#24634,#24635,#24636,#24637,#24638,
#24639,#24640,#24641,#24642,#24643,#24644,#24645,#24646,#24647,#24648,#24649,
#24650,#24651,#24652,#24653,#24654,#24655,#24656,#24657,#24658),
 .UNSPECIFIED.,.F.,.F.,(4,2,2,2,2,2,2,2,2,2,2,2,2,2,2,2,2,4),(-100.455361666765,
-100.170076029009,-99.8598933647241,-99.552143383566,-99.2372865599758,
-98.9295390353325,-98.6192902679461,-98.3071935852368,-98.0001977363163,
-97.6855532606439,-97.3760059671289,-97.0677518385104,-96.7535593223314,
-96.4461472340099,-96.134886301849,-95.8234121302857,-95.5162222726446,
-95.4519283393931),.UNSPECIFIED.);
#328=B_SPLINE_CURVE_WITH_KNOTS('',3,(#24663,#24664,#24665,#24666,#24667,
#24668,#24669,#24670,#24671,#24672,#24673,#24674,#24675,#24676,#24677,#24678,
#24679,#24680,#24681,#24682,#24683,#24684,#24685,#24686,#24687,#24688,#24689,
#24690,#24691,#24692,#24693,#24694,#24695,#24696,#24697,#24698),
 .UNSPECIFIED.,.F.,.F.,(4,2,2,2,2,2,2,2,2,2,2,2,2,2,2,2,2,4),(-17.0471773480641,
-16.858831398655,-16.5469160471412,-16.2392734228736,-15.9249731659921,
-15.6162249090113,-15.3065668667821,-14.9911686850119,-14.6838364190402,
-14.3716502905428,-14.060796004546,-13.7528833607647,-13.437947332658,-13.1297597759444,
-12.8194921961025,-12.5054502022621,-12.1981827248202,-12.038757850411),
 .UNSPECIFIED.);
#329=B_SPLINE_CURVE_WITH_KNOTS('',3,(#24699,#24700,#24701,#24702,#24703,
#24704,#24705,#24706,#24707,#24708,#24709,#24710,#24711,#24712,#24713,#24714,
#24715,#24716,#24717,#24718,#24719,#24720,#24721,#24722,#24723,#24724,#24725,
#24726,#24727,#24728,#24729,#24730,#24731,#24732,#24733,#24734),
 .UNSPECIFIED.,.F.,.F.,(4,2,2,2,2,2,2,2,2,2,2,2,2,2,2,2,2,4),(-95.4519283393931,
-95.2001303583947,-94.8911288140346,-94.5822053411759,-94.2685786867721,
-93.9612985535358,-93.6488915867085,-93.3379369392675,-93.030377939059,
-92.7147134772413,-92.4063569027996,-92.0967869846843,-91.7839183337999,
-91.4768183345611,-91.1632878409301,-90.85303324059,-90.5451455491716,-90.4465923804445),
 .UNSPECIFIED.);
#330=B_SPLINE_CURVE_WITH_KNOTS('',3,(#24739,#24740,#24741,#24742,#24743,
#24744,#24745,#24746,#24747,#24748,#24749,#24750,#24751,#24752,#24753,#24754,
#24755,#24756,#24757,#24758,#24759,#24760,#24761,#24762,#24763,#24764,#24765,
#24766,#24767,#24768,#24769,#24770,#24771,#24772,#24773,#24774),
 .UNSPECIFIED.,.F.,.F.,(4,2,2,2,2,2,2,2,2,2,2,2,2,2,2,2,2,4),(-22.0548538324586,
-21.832827853436,-21.5187457875705,-21.2115252632328,-20.8987529717923,
-20.5887876674696,-20.2804855806856,-19.9649278030172,-19.6571448681826,
-19.3462865382462,-19.0333952627533,-18.7260574772503,-18.4125437773414,
-18.1032938823081,-17.7943433300796,-17.4780103234481,-17.170425145641,
-17.0471773480641),.UNSPECIFIED.);
#331=B_SPLINE_CURVE_WITH_KNOTS('',3,(#24775,#24776,#24777,#24778,#24779,
#24780,#24781,#24782,#24783,#24784,#24785,#24786,#24787,#24788,#24789,#24790,
#24791,#24792,#24793,#24794,#24795,#24796,#24797,#24798,#24799,#24800,#24801,
#24802,#24803,#24804,#24805,#24806,#24807,#24808,#24809,#24810),
 .UNSPECIFIED.,.F.,.F.,(4,2,2,2,2,2,2,2,2,2,2,2,2,2,2,2,2,4),(-90.4465923804445,
-90.2302170891205,-89.9223838493343,-89.6119648299085,-89.299795102601,
-88.9926809815866,-88.6778369847466,-88.3682131269476,-88.0598102421047,
-87.7455409623599,-87.4380307810344,-87.1265897630268,-86.8150371043751,
-86.5077175775081,-86.1914185238541,-85.8823344459644,-85.573252838895,
-85.4407846201475),.UNSPECIFIED.);
#332=B_SPLINE_CURVE_WITH_KNOTS('',3,(#24815,#24816,#24817,#24818,#24819,
#24820,#24821,#24822,#24823,#24824,#24825,#24826,#24827,#24828,#24829,#24830,
#24831,#24832,#24833,#24834,#24835,#24836,#24837,#24838,#24839,#24840,#24841,
#24842,#24843,#24844,#24845,#24846,#24847,#24848,#24849,#24850),
 .UNSPECIFIED.,.F.,.F.,(4,2,2,2,2,2,2,2,2,2,2,2,2,2,2,2,2,4),(-27.0628130182279,
-26.8069778864524,-26.490730231184,-26.1831669347654,-25.8716551853357,
-25.559709422747,-25.2521228733781,-24.9379080994133,-24.6291615235746,
-24.3195868347493,-24.0041384835497,-23.6968401183334,-23.3847428143161,
-23.0738674443347,-22.7660247078664,-22.4511806787902,-22.1430061561745,
-22.0548538324586),.UNSPECIFIED.);
#333=B_SPLINE_CURVE_WITH_KNOTS('',3,(#24851,#24852,#24853,#24854,#24855,
#24856,#24857,#24858,#24859,#24860,#24861,#24862,#24863,#24864,#24865,#24866,
#24867,#24868,#24869,#24870,#24871,#24872,#24873,#24874,#24875,#24876,#24877,
#24878,#24879,#24880,#24881,#24882,#24883,#24884,#24885,#24886),
 .UNSPECIFIED.,.F.,.F.,(4,2,2,2,2,2,2,2,2,2,2,2,2,2,2,2,2,4),(-85.4407846201475,
-85.2595428973909,-84.9521525010805,-84.639558343424,-84.3285184262725,
-84.0208197185399,-83.705070310243,-83.3966229683412,-83.0868823718611,
-82.7739279078785,-82.4667066598592,-82.1529764130471,-81.8426333927081,
-81.5345946694503,-81.2195777462055,-80.911642722096,-80.601041703004,-80.4335177250807),
 .UNSPECIFIED.);
#334=B_SPLINE_CURVE_WITH_KNOTS('',3,(#24891,#24892,#24893,#24894,#24895,
#24896,#24897,#24898,#24899,#24900,#24901,#24902,#24903,#24904,#24905,#24906,
#24907,#24908,#24909,#24910,#24911,#24912,#24913,#24914,#24915,#24916,#24917,
#24918,#24919,#24920,#24921,#24922,#24923,#24924,#24925,#24926),
 .UNSPECIFIED.,.F.,.F.,(4,2,2,2,2,2,2,2,2,2,2,2,2,2,2,2,2,4),(-32.0696198736087,
-31.7781082037164,-31.4633407311828,-31.1551614995253,-30.8450572548339,
-30.5309155756559,-30.2237251951323,-29.9110318438284,-29.6010389747784,
-29.2928044075254,-28.9773283521885,-28.6695537841855,-28.3587741699972,
-28.0458367711374,-27.7385425892498,-27.4251117737632,-27.1158485377647,
-27.0628130182279),.UNSPECIFIED.);
#335=B_SPLINE_CURVE_WITH_KNOTS('',3,(#24927,#24928,#24929,#24930,#24931,
#24932,#24933,#24934,#24935,#24936,#24937,#24938,#24939,#24940,#24941,#24942,
#24943,#24944,#24945,#24946,#24947,#24948,#24949,#24950,#24951,#24952,#24953,
#24954,#24955,#24956,#24957,#24958,#24959,#24960,#24961,#24962),
 .UNSPECIFIED.,.F.,.F.,(4,2,2,2,2,2,2,2,2,2,2,2,2,2,2,2,2,4),(-80.4335177250807,
-80.2887823377538,-79.9815356448999,-79.6664817246118,-79.3567650240283,
-79.0482006811451,-78.7338380395159,-78.4262143499005,-78.1145820896486,
-77.8029345943652,-77.4954717391251,-77.1790776601926,-76.8700744291997,
-76.5610545946566,-76.2474854347615,-75.9402037447504,-75.627644696357,
-75.4263375761454),.UNSPECIFIED.);
#336=B_SPLINE_CURVE_WITH_KNOTS('',3,(#24967,#24968,#24969,#24970,#24971,
#24972,#24973,#24974,#24975,#24976,#24977,#24978,#24979,#24980,#24981,#24982,
#24983,#24984,#24985,#24986,#24987,#24988,#24989,#24990,#24991,#24992,#24993,
#24994,#24995,#24996,#24997,#24998,#24999,#25000,#25001,#25002,#25003,#25004),
 .UNSPECIFIED.,.F.,.F.,(4,2,2,2,2,2,2,2,2,2,2,2,2,2,2,2,2,2,4),(-37.0769841873551,
-37.0575083077529,-36.7502407984738,-36.4368770759001,-36.1275822274484,
-35.8187752969543,-35.5025971161927,-35.1950383117034,-34.88359289563,-34.5715978566608,
-34.2640507816734,-33.9499057927643,-33.6411429317627,-33.331636141935,
-33.0161179680958,-32.7088363625265,-32.3968124814779,-32.0858972713141,
-32.0696198736087),.UNSPECIFIED.);
#337=B_SPLINE_CURVE_WITH_KNOTS('',3,(#25005,#25006,#25007,#25008,#25009,
#25010,#25011,#25012,#25013,#25014,#25015,#25016,#25017,#25018,#25019,#25020,
#25021,#25022,#25023,#25024,#25025,#25026,#25027,#25028,#25029,#25030,#25031,
#25032,#25033,#25034,#25035,#25036,#25037,#25038,#25039,#25040),
 .UNSPECIFIED.,.F.,.F.,(4,2,2,2,2,2,2,2,2,2,2,2,2,2,2,2,2,4),(-75.4263375761454,
-75.3167416267388,-75.0091222628059,-74.693513377888,-74.3851950606098,
-74.0755041712474,-73.7626873451246,-73.4555636200335,-73.1418568101527,
-72.831646908359,-72.5236764420255,-72.208795912533,-71.9009784300672,-71.5904164789951,
-71.2782903385179,-70.9711298391533,-70.6560902661978,-70.4207058556691),
 .UNSPECIFIED.);
#338=B_SPLINE_CURVE_WITH_KNOTS('',3,(#25045,#25046,#25047,#25048,#25049,
#25050,#25051,#25052,#25053,#25054,#25055,#25056,#25057,#25058,#25059,#25060,
#25061,#25062,#25063,#25064,#25065,#25066,#25067,#25068,#25069,#25070,#25071,
#25072,#25073,#25074,#25075,#25076,#25077,#25078,#25079,#25080),
 .UNSPECIFIED.,.F.,.F.,(4,2,2,2,2,2,2,2,2,2,2,2,2,2,2,2,2,4),(-42.0835650080859,
-42.0276024561896,-41.7203201695277,-41.4083535901313,-41.0973799381269,
-40.7896277028518,-40.4749206008968,-40.1667187871955,-39.8566726623258,
-39.5424521318403,-39.2352746747194,-38.922644324604,-38.6126054028072,
-38.3044218286954,-37.98901148703,-37.6812276180551,-37.37051094087,-37.0769841873551),
 .UNSPECIFIED.);
#339=B_SPLINE_CURVE_WITH_KNOTS('',3,(#25081,#25082,#25083,#25084,#25085,
#25086,#25087,#25088,#25089,#25090,#25091,#25092,#25093,#25094,#25095,#25096,
#25097,#25098,#25099,#25100,#25101,#25102,#25103,#25104,#25105,#25106,#25107,
#25108,#25109,#25110,#25111,#25112,#25113,#25114,#25115,#25116),
 .UNSPECIFIED.,.F.,.F.,(4,2,2,2,2,2,2,2,2,2,2,2,2,2,2,2,2,4),(-70.4207058556691,
-70.3465017244344,-70.0379956331957,-69.7237639236243,-69.416245783058,
-69.1046441997098,-68.7931241987137,-68.4857369618575,-68.1694742193023,
-67.8605977832699,-67.5516229712482,-67.2381825248866,-66.9309955834494,
-66.6184531943587,-66.3076748184943,-66.0001191746988,-65.684638545429,
-65.4152002552604),.UNSPECIFIED.);
#340=B_SPLINE_CURVE_WITH_KNOTS('',3,(#25121,#25122,#25123,#25124,#25125,
#25126,#25127,#25128,#25129,#25130,#25131,#25132,#25133,#25134,#25135,#25136,
#25137,#25138,#25139,#25140,#25141,#25142,#25143,#25144,#25145,#25146,#25147,
#25148,#25149,#25150,#25151,#25152,#25153,#25154,#25155,#25156),
 .UNSPECIFIED.,.F.,.F.,(4,2,2,2,2,2,2,2,2,2,2,2,2,2,2,2,2,4),(-47.0910467575489,
-47.0004773013202,-46.692666388461,-46.3819962211513,-46.0689096299662,
-45.7616514853505,-45.4483383831922,-45.138993755588,-44.8302336827447,
-44.514108399339,-44.206536503736,-43.8951410858116,-43.5830781495772,-43.2755534665247,
-42.9614618670812,-42.6526647270027,-42.3432097035513,-42.0835650080859),
 .UNSPECIFIED.);
#341=B_SPLINE_CURVE_WITH_KNOTS('',3,(#25157,#25158,#25159,#25160,#25161,
#25162,#25163,#25164,#25165,#25166,#25167,#25168,#25169,#25170,#25171,#25172,
#25173,#25174,#25175,#25176,#25177,#25178,#25179,#25180,#25181,#25182,#25183,
#25184,#25185,#25186,#25187,#25188,#25189,#25190,#25191,#25192),
 .UNSPECIFIED.,.F.,.F.,(4,2,2,2,2,2,2,2,2,2,2,2,2,2,2,2,2,4),(-65.4152002552604,
-65.376436341034,-65.0667777641196,-64.7540863074667,-64.4470455058427,
-64.1333431058225,-63.8232539322029,-63.5153355089084,-63.200578841122,
-62.8928653273433,-62.5823245298298,-62.2703190625795,-61.9632295532419,
-61.6481849043275,-61.3387118184057,-61.0302472735284,-60.7161336210183,
-60.4108627972263),.UNSPECIFIED.);
#342=B_SPLINE_CURVE_WITH_KNOTS('',3,(#25197,#25198,#25199,#25200,#25201,
#25202,#25203,#25204,#25205,#25206,#25207,#25208,#25209,#25210,#25211,#25212,
#25213,#25214,#25215,#25216,#25217,#25218,#25219,#25220,#25221,#25222,#25223,
#25224,#25225,#25226,#25227,#25228,#25229,#25230,#25231,#25232),
 .UNSPECIFIED.,.F.,.F.,(4,2,2,2,2,2,2,2,2,2,2,2,2,2,2,2,2,4),(-52.0980129685988,
-51.9730797155729,-51.6642304507307,-51.3548104950973,-51.0390955345897,
-50.7317949854421,-50.4198689750653,-50.108818627249,-49.8010859273223,
-49.4864223734463,-49.1781801469801,-48.8681755897101,-48.5538574830228,
-48.2466754690557,-47.9340915292134,-47.6239883003567,-47.3158386130918,
-47.0910467575489),.UNSPECIFIED.);
#343=B_SPLINE_CURVE_WITH_KNOTS('',3,(#25233,#25234,#25235,#25236,#25237,
#25238,#25239,#25240,#25241,#25242,#25243,#25244,#25245,#25246,#25247,#25248,
#25249,#25250,#25251,#25252,#25253,#25254,#25255,#25256,#25257,#25258,#25259,
#25260,#25261,#25262,#25263,#25264,#25265,#25266,#25267,#25268,#25269,#25270),
 .UNSPECIFIED.,.F.,.F.,(4,2,2,2,2,2,2,2,2,2,2,2,2,2,2,2,2,2,4),(-60.4108627972263,
-60.4087068158386,-60.0971176296951,-59.7857122133521,-59.4783848698016,
-59.1622404359523,-58.8534775234458,-58.5445303791034,-58.2312056492169,
-57.9240986618394,-57.6115540159792,-57.300887267302,-56.9933790350214,
-56.6780134555657,-56.3699135075542,-56.0602693186155,-55.7476900387188,
-55.4407167803585,-55.4071129852565),.UNSPECIFIED.);
#344=B_SPLINE_CURVE_WITH_KNOTS('',3,(#25275,#25276,#25277,#25278,#25279,
#25280,#25281,#25282,#25283,#25284,#25285,#25286,#25287,#25288,#25289,#25290,
#25291,#25292,#25293,#25294,#25295,#25296,#25297,#25298,#25299,#25300,#25301,
#25302,#25303,#25304,#25305,#25306,#25307,#25308,#25309,#25310),
 .UNSPECIFIED.,.F.,.F.,(4,2,2,2,2,2,2,2,2,2,2,2,2,2,2,2,2,4),(-57.1054920760842,
-56.9437704025751,-56.6365568449243,-56.322735716271,-56.0124454172078,
-55.7043761272089,-55.3937355145563,-55.0805468237212,-54.7732805137774,
-54.4600009967079,-54.1505887093072,-53.8418580853489,-53.5257685396563,
-53.2181659400515,-52.9068036303523,-52.5946546131302,-52.2871349042509,
-52.0980129685988),.UNSPECIFIED.);
#345=B_SPLINE_CURVE_WITH_KNOTS('',3,(#25311,#25312,#25313,#25314,#25315,
#25316,#25317,#25318,#25319,#25320,#25321,#25322,#25323,#25324,#25325,#25326,
#25327,#25328,#25329,#25330,#25331,#25332,#25333,#25334,#25335,#25336,#25337,
#25338,#25339,#25340,#25341,#25342,#25343,#25344,#25345,#25346),
 .UNSPECIFIED.,.F.,.F.,(4,2,2,2,2,2,2,2,2,2,2,2,2,2,2,2,2,4),(-55.4071129852565,
-55.1269993808329,-54.8170176401417,-54.5091344278048,-54.194488160584,
-53.8868641521749,-53.5763261395185,-53.2644278801274,-52.9573934420036,
-52.6423239878026,-52.3329527642613,-52.0245125101988,-51.7105031272677,
-51.4031526194724,-51.0958326655231,-50.7819027279722,-50.4733999003014,
-50.4034127968505),.UNSPECIFIED.);
#346=B_SPLINE_CURVE_WITH_KNOTS('',3,(#25351,#25352,#25353,#25354,#25355,
#25356,#25357,#25358,#25359,#25360,#25361,#25362,#25363,#25364,#25365,#25366,
#25367,#25368,#25369,#25370,#25371,#25372,#25373,#25374,#25375,#25376,#25377,
#25378,#25379,#25380,#25381,#25382,#25383,#25384,#25385,#25386),
 .UNSPECIFIED.,.F.,.F.,(4,2,2,2,2,2,2,2,2,2,2,2,2,2,2,2,2,4),(-62.1136210401049,
-61.9163387340731,-61.6086313703946,-61.2968929557857,-60.9851664195768,
-60.6776115528275,-60.3611377639058,-60.0520563158807,-59.7429353108473,
-59.4292867469164,-59.1219184839582,-58.8092489948486,-58.4982663785463,
-58.1905516047176,-57.8748624413629,-57.5664631706967,-57.2566672869653,
-57.1054920760842),.UNSPECIFIED.);
#347=B_SPLINE_CURVE_WITH_KNOTS('',3,(#25387,#25388,#25389,#25390,#25391,
#25392,#25393,#25394,#25395,#25396,#25397,#25398,#25399,#25400,#25401,#25402,
#25403,#25404,#25405,#25406,#25407,#25408,#25409,#25410,#25411,#25412,#25413,
#25414,#25415,#25416,#25417,#25418,#25419,#25420,#25421,#25422),
 .UNSPECIFIED.,.F.,.F.,(4,2,2,2,2,2,2,2,2,2,2,2,2,2,2,2,2,4),(-50.4034127968505,
-50.164105472623,-49.8488834773958,-49.5418417861919,-49.230029139742,-48.9193892122316,
-48.6118193294818,-48.297263519743,-47.9893372298427,-47.6794422899663,
-47.3655898524267,-47.058631647327,-46.7461468985924,-46.4364215495851,
-46.1283985834444,-45.8131317920273,-45.5056023522412,-45.4002962379396),
 .UNSPECIFIED.);
#348=B_SPLINE_CURVE_WITH_KNOTS('',3,(#25427,#25428,#25429,#25430,#25431,
#25432,#25433,#25434,#25435,#25436,#25437,#25438,#25439,#25440,#25441,#25442,
#25443,#25444,#25445,#25446,#25447,#25448,#25449,#25450,#25451,#25452,#25453,
#25454,#25455,#25456,#25457,#25458,#25459,#25460,#25461,#25462),
 .UNSPECIFIED.,.F.,.F.,(4,2,2,2,2,2,2,2,2,2,2,2,2,2,2,2,2,4),(-67.1222250534393,
-66.8889859665686,-66.5804612178844,-66.2706205210999,-65.9575893611776,
-65.6502823358052,-65.3364431537315,-65.0260231367163,-64.7178901318218,
-64.4027954105073,-64.0947799572192,-63.7840755293362,-63.4717384956288,
-63.1644028402809,-62.8492369333942,-62.5394420846956,-62.2307804551113,
-62.1136210401049),.UNSPECIFIED.);
#349=B_SPLINE_CURVE_WITH_KNOTS('',3,(#25463,#25464,#25465,#25466,#25467,
#25468,#25469,#25470,#25471,#25472,#25473,#25474,#25475,#25476,#25477,#25478,
#25479,#25480,#25481,#25482,#25483,#25484,#25485,#25486,#25487,#25488,#25489,
#25490,#25491,#25492,#25493,#25494,#25495,#25496,#25497,#25498),
 .UNSPECIFIED.,.F.,.F.,(4,2,2,2,2,2,2,2,2,2,2,2,2,2,2,2,2,4),(-45.4002962379396,
-45.1950299093757,-44.8823730677161,-44.5753034279609,-44.2620795406819,
-43.9530750929825,-43.644409446872,-43.3283695899486,-43.0210435048463,
-42.7097376296218,-42.398062628467,-42.0906936991598,-41.7766849905124,
-41.4681881765344,-41.1588170036172,-40.8436536045709,-40.5365853475107,
-40.3961502328463),.UNSPECIFIED.);
#350=B_SPLINE_CURVE_WITH_KNOTS('',3,(#25503,#25504,#25505,#25506,#25507,
#25508,#25509,#25510,#25511,#25512,#25513,#25514,#25515,#25516,#25517,#25518,
#25519,#25520,#25521,#25522,#25523,#25524,#25525,#25526,#25527,#25528,#25529,
#25530,#25531,#25532,#25533,#25534,#25535,#25536,#25537,#25538),
 .UNSPECIFIED.,.F.,.F.,(4,2,2,2,2,2,2,2,2,2,2,2,2,2,2,2,2,4),(-72.1302573428804,
-71.8631304122031,-71.5534330563933,-71.2449364392317,-70.9305928217517,
-70.6230033389037,-70.3114592540741,-69.9998322224352,-69.6924245282241,
-69.3760139851406,-69.0668548000318,-68.7576767210128,-68.443890679124,
-68.1364175726176,-67.8237181807294,-67.5126020479389,-67.2048122935097,
-67.1222250534393),.UNSPECIFIED.);
#351=B_SPLINE_CURVE_WITH_KNOTS('',3,(#25539,#25540,#25541,#25542,#25543,
#25544,#25545,#25546,#25547,#25548,#25549,#25550,#25551,#25552,#25553,#25554,
#25555,#25556,#25557,#25558,#25559,#25560,#25561,#25562,#25563,#25564,#25565,
#25566,#25567,#25568,#25569,#25570,#25571,#25572,#25573,#25574),
 .UNSPECIFIED.,.F.,.F.,(4,2,2,2,2,2,2,2,2,2,2,2,2,2,2,2,2,4),(-40.3961502328463,
-40.2246904616579,-39.9140796544823,-39.606446806267,-39.2918055999392,
-38.9838738720454,-38.6738961625095,-38.3600921718419,-38.053094203686,
-37.7405218252869,-37.4308134458335,-37.1227139008544,-36.8073566670787,
-36.4998088910576,-36.1891491286477,-35.8765273825777,-35.5694047444726,
-35.3924138450891),.UNSPECIFIED.);
#352=B_SPLINE_CURVE_WITH_KNOTS('',3,(#25579,#25580,#25581,#25582,#25583,
#25584,#25585,#25586,#25587,#25588,#25589,#25590,#25591,#25592,#25593,#25594,
#25595,#25596,#25597,#25598,#25599,#25600,#25601,#25602,#25603,#25604,#25605,
#25606,#25607,#25608,#25609,#25610,#25611,#25612,#25613,#25614),
 .UNSPECIFIED.,.F.,.F.,(4,2,2,2,2,2,2,2,2,2,2,2,2,2,2,2,2,4),(-77.1366478717291,
-76.8355230676794,-76.5244969661853,-76.2168508494848,-75.9011143340131,
-75.5926850995749,-75.2830185434786,-74.9700779966474,-74.6628964476979,
-74.3492600632362,-74.0389331812871,-73.7309549479999,-73.4159535036981,
-73.1080444062249,-72.7975252397004,-72.4852825886811,-72.178083541516,
-72.1302573428804),.UNSPECIFIED.);
#353=B_SPLINE_CURVE_WITH_KNOTS('',3,(#25615,#25616,#25617,#25618,#25619,
#25620,#25621,#25622,#25623,#25624,#25625,#25626,#25627,#25628,#25629,#25630,
#25631,#25632,#25633,#25634,#25635,#25636,#25637,#25638,#25639,#25640,#25641,
#25642,#25643,#25644,#25645,#25646,#25647,#25648,#25649,#25650),
 .UNSPECIFIED.,.F.,.F.,(4,2,2,2,2,2,2,2,2,2,2,2,2,2,2,2,2,4),(-35.3924138450891,
-35.2560893785116,-34.9470878667756,-34.6383335093246,-34.3221996684171,
-34.014841951678,-33.7034455514833,-33.3917901474578,-33.0843559896569,
-32.7702532653614,-32.461744606947,-32.1522816756052,-31.8371571040235,
-31.5300453916212,-31.2180533276116,-30.9074528993813,-30.5997412551407,
-30.3874064632604),.UNSPECIFIED.);
#354=B_SPLINE_CURVE_WITH_KNOTS('',3,(#25655,#25656,#25657,#25658,#25659,
#25660,#25661,#25662,#25663,#25664,#25665,#25666,#25667,#25668,#25669,#25670,
#25671,#25672,#25673,#25674,#25675,#25676,#25677,#25678,#25679,#25680,#25681,
#25682,#25683,#25684,#25685,#25686,#25687,#25688,#25689,#25690,#25691,#25692),
 .UNSPECIFIED.,.F.,.F.,(4,2,2,2,2,2,2,2,2,2,2,2,2,2,2,2,2,2,4),(-82.1419590834687,
-82.1176007910994,-81.8072554425438,-81.4950907524697,-81.1880142579156,
-80.873263839072,-80.5636478744585,-80.2553038443901,-79.9410419117584,
-79.633555116795,-79.3221945146972,-79.0106508199037,-78.703376894399,-78.387176536406,
-78.0781046361535,-77.7690883629183,-77.4553904456565,-77.1480320043487,
-77.1366478717291),.UNSPECIFIED.);
#355=B_SPLINE_CURVE_WITH_KNOTS('',3,(#25693,#25694,#25695,#25696,#25697,
#25698,#25699,#25700,#25701,#25702,#25703,#25704,#25705,#25706,#25707,#25708,
#25709,#25710,#25711,#25712,#25713,#25714,#25715,#25716,#25717,#25718,#25719,
#25720,#25721,#25722,#25723,#25724,#25725,#25726,#25727,#25728),
 .UNSPECIFIED.,.F.,.F.,(4,2,2,2,2,2,2,2,2,2,2,2,2,2,2,2,2,4),(-30.3874064632604,
-30.2849996850917,-29.9770449392946,-29.6669697019036,-29.3531945565624,
-29.0461403261237,-28.7334656171847,-28.4237557504156,-28.1155642693923,
-27.800101850319,-27.4925185322491,-27.1817568932496,-26.8691509574993,
-26.5619592729381,-26.2485379032423,-25.9395212737839,-25.6306633294113,
-25.3825818071783),.UNSPECIFIED.);
#356=B_SPLINE_CURVE_WITH_KNOTS('',3,(#25733,#25734,#25735,#25736,#25737,
#25738,#25739,#25740,#25741,#25742,#25743,#25744,#25745,#25746,#25747,#25748,
#25749,#25750,#25751,#25752,#25753,#25754,#25755,#25756,#25757,#25758,#25759,
#25760,#25761,#25762,#25763,#25764,#25765,#25766,#25767,#25768),
 .UNSPECIFIED.,.F.,.F.,(4,2,2,2,2,2,2,2,2,2,2,2,2,2,2,2,2,4),(-87.1467179399563,
-87.08588220081,-86.7770149001574,-86.4633883814524,-86.156129319966,-85.8437993712712,
-85.5328468320979,-85.2253306548538,-84.909667125882,-84.6013169568405,
-84.2918124156487,-83.9789458786145,-83.6718751054293,-83.3584307994978,
-83.0481807364898,-82.7403442197742,-82.425419395495,-82.1419590834687),
 .UNSPECIFIED.);
#357=B_SPLINE_CURVE_WITH_KNOTS('',3,(#25769,#25770,#25771,#25772,#25773,
#25774,#25775,#25776,#25777,#25778,#25779,#25780,#25781,#25782,#25783,#25784,
#25785,#25786,#25787,#25788,#25789,#25790,#25791,#25792,#25793,#25794,#25795,
#25796,#25797,#25798,#25799,#25800,#25801,#25802,#25803,#25804),
 .UNSPECIFIED.,.F.,.F.,(4,2,2,2,2,2,2,2,2,2,2,2,2,2,2,2,2,4),(-25.3825818071783,
-25.3144209224753,-25.0070148119768,-24.695513470675,-24.3838588306673,
-24.0763438668322,-23.7621327140135,-23.4535946485024,-23.1440257555464,
-22.8289201864819,-22.5217486530133,-22.2096453156183,-21.8990366757631,
-21.5912311755097,-21.2763751382008,-20.9683801793135,-20.6581934941524,
-20.3765334205341),.UNSPECIFIED.);
#358=B_SPLINE_CURVE_WITH_KNOTS('',3,(#25809,#25810,#25811,#25812,#25813,
#25814,#25815,#25816,#25817,#25818,#25819,#25820,#25821,#25822,#25823,#25824,
#25825,#25826,#25827,#25828,#25829,#25830,#25831,#25832,#25833,#25834,#25835,
#25836,#25837,#25838,#25839,#25840,#25841,#25842,#25843,#25844),
 .UNSPECIFIED.,.F.,.F.,(4,2,2,2,2,2,2,2,2,2,2,2,2,2,2,2,2,4),(-92.1499753716227,
-92.0541924144739,-91.7464836512906,-91.4316182443593,-91.123873592165,
-90.8136895664306,-90.5015858623512,-90.1946170421438,-89.8800580960553,
-89.5705068478487,-89.2623020321016,-88.9481047839233,-88.6407047453379,
-88.3295157048067,-88.0180385885635,-87.7108841615196,-87.3948832438076,
-87.1467179399563),.UNSPECIFIED.);
#359=B_SPLINE_CURVE_WITH_KNOTS('',3,(#25845,#25846,#25847,#25848,#25849,
#25850,#25851,#25852,#25853,#25854,#25855,#25856,#25857,#25858,#25859,#25860,
#25861,#25862,#25863,#25864,#25865,#25866,#25867,#25868,#25869,#25870,#25871,
#25872,#25873,#25874,#25875,#25876,#25877,#25878,#25879,#25880,#25881,#25882),
 .UNSPECIFIED.,.F.,.F.,(4,2,2,2,2,2,2,2,2,2,2,2,2,2,2,2,2,2,4),(-20.3765334205341,
-20.3444276288399,-20.0373012529877,-19.7245103792346,-19.4147808169846,
-19.1064828976576,-18.7909014347054,-18.4832658461886,-18.1723886302269,
-17.859779364247,-17.5525032859371,-17.2389622676149,-16.929912818555,-16.6209373331314,
-16.3045726743746,-15.9971019731104,-15.6854821421927,-15.373809691922,
-15.3702501983023),.UNSPECIFIED.);
#360=B_SPLINE_CURVE_WITH_KNOTS('',3,(#25887,#25888,#25889,#25890,#25891,
#25892,#25893,#25894,#25895,#25896,#25897,#25898,#25899,#25900,#25901,#25902,
#25903,#25904,#25905,#25906,#25907,#25908,#25909,#25910,#25911,#25912,#25913,
#25914,#25915,#25916,#25917,#25918,#25919,#25920,#25921,#25922),
 .UNSPECIFIED.,.F.,.F.,(4,2,2,2,2,2,2,2,2,2,2,2,2,2,2,2,2,4),(-97.1531123408846,
-97.0224344199092,-96.7153844107451,-96.3995709672319,-96.0906238614074,
-95.7818917441421,-95.468319396795,-95.1611437241807,-94.848980193566,-94.5380842326777,
-94.230683440607,-93.9150755558694,-93.6067873912186,-93.2974317275935,
-92.9846220740555,-92.6776466084498,-92.3643825150026,-92.1499753716227),
 .UNSPECIFIED.);
#361=B_SPLINE_CURVE_WITH_KNOTS('',3,(#25923,#25924,#25925,#25926,#25927,
#25928,#25929,#25930,#25931,#25932,#25933,#25934,#25935,#25936,#25937,#25938,
#25939,#25940,#25941,#25942,#25943,#25944,#25945,#25946,#25947,#25948,#25949,
#25950,#25951,#25952,#25953,#25954,#25955,#25956,#25957,#25958),
 .UNSPECIFIED.,.F.,.F.,(4,2,2,2,2,2,2,2,2,2,2,2,2,2,2,2,2,4),(-15.3702501983023,
-15.0661991157021,-14.7518660086767,-14.4432814244333,-14.1335932317505,
-13.8184870007477,-13.5112399241302,-13.199012110835,-12.8883770031141,
-12.5804634365136,-12.2654797384413,-11.9574278997467,-11.6471167320135,
-11.3333408258675,-11.0261271421597,-10.713207177595,-10.4034401316373,
-10.3632048196668),.UNSPECIFIED.);
#362=B_SPLINE_CURVE_WITH_KNOTS('',3,(#25963,#25964,#25965,#25966,#25967,
#25968,#25969,#25970,#25971,#25972,#25973,#25974,#25975,#25976,#25977,#25978,
#25979,#25980,#25981,#25982,#25983,#25984,#25985,#25986,#25987,#25988,#25989,
#25990,#25991,#25992,#25993,#25994,#25995,#25996,#25997,#25998),
 .UNSPECIFIED.,.F.,.F.,(4,2,2,2,2,2,2,2,2,2,2,2,2,2,2,2,2,4),(-102.154690645213,
-101.987556999368,-101.680660695609,-101.367563783602,-101.057416380731,
-100.749820529465,-100.434996927783,-100.127309127348,-99.8172728811381,
-99.5052127675913,-99.1983359936896,-98.8839560771392,-98.5744524240466,
-98.2663725330835,-97.9522225174849,-97.6448926661825,-97.3338621803013,
-97.1531123408846),.UNSPECIFIED.);
#363=B_SPLINE_CURVE_WITH_KNOTS('',3,(#25999,#26000,#26001,#26002,#26003,
#26004,#26005,#26006,#26007,#26008,#26009,#26010,#26011,#26012,#26013,#26014,
#26015,#26016,#26017,#26018,#26019,#26020,#26021,#26022,#26023,#26024,#26025,
#26026,#26027,#26028,#26029,#26030,#26031,#26032,#26033,#26034),
 .UNSPECIFIED.,.F.,.F.,(4,2,2,2,2,2,2,2,2,2,2,2,2,2,2,2,2,4),(-10.3632048196668,
-10.0950221884295,-9.77930874677035,-9.47160476592912,-9.16059916985077,
-8.84796777245071,-8.54059274199171,-8.22691934660563,-7.91781988331396,
-7.6087138693961,-7.29221420374721,-6.98466339271854,-6.67291242750295,
-6.36120402867725,-6.05348387685949,-5.73901621000068,-5.43036858402126,
-5.35481643806797),.UNSPECIFIED.);
#364=B_SPLINE_CURVE_WITH_KNOTS('',3,(#26041,#26042,#26043,#26044,#26045,
#26046,#26047,#26048,#26049,#26050,#26051,#26052,#26053,#26054,#26055,#26056,
#26057,#26058,#26059,#26060,#26061,#26062,#26063,#26064,#26065,#26066,#26067,
#26068,#26069,#26070,#26071,#26072,#26073,#26074),.UNSPECIFIED.,.F.,.F.,
(4,2,2,2,2,2,2,2,2,2,2,2,2,2,2,2,4),(-106.874476063165,-106.604105121065,
-106.335692503319,-106.024296620534,-105.717335282747,-105.401696172039,
-105.092785792685,-104.784174219368,-104.470638521187,-104.163529711546,
-103.851518994257,-103.540662313851,-103.233361625802,-102.917791732759,
-102.609548098789,-102.300327250781,-102.154690645213),.UNSPECIFIED.);
#365=B_SPLINE_CURVE_WITH_KNOTS('',3,(#26075,#26076,#26077,#26078,#26079,
#26080,#26081,#26082,#26083,#26084,#26085,#26086,#26087,#26088,#26089,#26090,
#26091,#26092,#26093,#26094,#26095,#26096,#26097,#26098,#26099,#26100,#26101,
#26102,#26103,#26104,#26105,#26106,#26107,#26108,#26109,#26110),
 .UNSPECIFIED.,.F.,.F.,(4,2,2,2,2,2,2,2,2,2,2,2,2,2,2,2,2,4),(-5.35481643806797,
-5.12054865168396,-4.80542245821637,-4.49808485837619,-4.18572028641412,
-3.87504095581268,-3.56700601646214,-3.25188239828953,-2.94375766551306,
-2.63330989072761,-2.31950505958809,-2.01218970805026,-1.69912865491474,
-1.38930690941913,-1.08075630985562,-0.764898895970032,-0.457111115329854,
-0.346239220973872),.UNSPECIFIED.);
#366=B_SPLINE_CURVE_WITH_KNOTS('',3,(#26136,#26137,#26138,#26139,#26140,
#26141,#26142,#26143,#26144,#26145,#26146,#26147,#26148,#26149,#26150,#26151,
#26152,#26153,#26154,#26155,#26156,#26157,#26158,#26159,#26160,#26161,#26162,
#26163,#26164,#26165,#26166,#26167,#26168,#26169,#26170,#26171,#26172,#26173,
#26174,#26175,#26176,#26177,#26178,#26179,#26180,#26181,#26182,#26183,#26184,
#26185,#26186,#26187,#26188,#26189,#26190,#26191,#26192,#26193,#26194,#26195,
#26196,#26197,#26198,#26199,#26200,#26201,#26202),.UNSPECIFIED.,.F.,.F.,
(4,3,3,3,3,3,3,3,3,3,3,3,3,3,3,3,3,3,3,3,3,3,4),(0.0041660518496644,0.00459976416699748,
0.00546021591375608,0.0057750006243275,0.00639487133587175,0.00675437997785038,
0.00695961430893405,0.00757842774990045,0.00804854404194467,0.0081494048247967,
0.00869562607399181,0.00874625427688977,0.00920849047335839,0.00934270810603896,
0.00934406861977701,0.0106292804107923,0.0117265310038454,0.0119310362342275,
0.0125368230564803,0.0129107735164763,0.0132252002983218,0.0140854315246815,
0.0145193643624109),.UNSPECIFIED.);
#367=B_SPLINE_CURVE_WITH_KNOTS('',3,(#26203,#26204,#26205,#26206,#26207,
#26208,#26209,#26210,#26211,#26212,#26213,#26214,#26215,#26216,#26217,#26218,
#26219,#26220,#26221,#26222,#26223,#26224,#26225,#26226,#26227,#26228,#26229,
#26230,#26231,#26232,#26233,#26234,#26235,#26236,#26237,#26238,#26239,#26240,
#26241,#26242,#26243,#26244,#26245,#26246,#26247,#26248,#26249,#26250,#26251,
#26252,#26253,#26254,#26255,#26256,#26257,#26258,#26259,#26260,#26261,#26262,
#26263,#26264,#26265,#26266,#26267,#26268,#26269),.UNSPECIFIED.,.F.,.F.,
(4,3,3,3,3,3,3,3,3,3,3,3,3,3,3,3,3,3,3,3,3,3,4),(0.0041660518496669,0.0045997641669973,
0.00546021591375601,0.00577500062432757,0.00639487133588581,0.00675437997785032,
0.0069596143089341,0.00757842774983116,0.00804854404194462,0.00814940482479665,
0.00869562607399177,0.00874625427688975,0.00920849047333203,0.00934270810603892,
0.00934406861977701,0.0106292804114527,0.0117265310038455,0.0119310362342275,
0.0125368230564929,0.0129107735164765,0.0132252002983218,0.0140854315246816,
0.0145193643624118),.UNSPECIFIED.);
#368=B_SPLINE_CURVE_WITH_KNOTS('',3,(#26271,#26272,#26273,#26274,#26275,
#26276,#26277,#26278,#26279,#26280,#26281,#26282,#26283,#26284),
 .UNSPECIFIED.,.F.,.F.,(4,2,2,2,2,2,4),(-1.62358010524267,-1.32771579098637,
-1.0654737946073,-0.587083880817408,-0.264803320204801,-0.13597564184897,
0.),.UNSPECIFIED.);
#369=B_SPLINE_CURVE_WITH_KNOTS('',3,(#26288,#26289,#26290,#26291,#26292,
#26293,#26294,#26295,#26296,#26297,#26298,#26299,#26300,#26301,#26302,#26303,
#26304,#26305),.UNSPECIFIED.,.F.,.F.,(4,2,2,2,2,2,2,2,4),(-3.97757183645169,
-3.73001710320254,-3.47073400331661,-3.19180345145064,-2.83616150801241,
-2.51533726294721,-2.3691450825456,-2.0816506234592,-1.94059934416272),
 .UNSPECIFIED.);
#370=B_SPLINE_CURVE_WITH_KNOTS('',3,(#26309,#26310,#26311,#26312,#26313,
#26314,#26315,#26316,#26317,#26318,#26319,#26320,#26321,#26322,#26323,#26324,
#26325,#26326),.UNSPECIFIED.,.F.,.F.,(4,2,2,2,2,2,2,2,4),(-1.94059934416272,
-1.80303531466732,-1.51989931485796,-1.21685973325026,-0.90441123218411,
-0.606202781914648,-0.343816058000839,-0.168665484648542,0.),
 .UNSPECIFIED.);
#371=B_SPLINE_CURVE_WITH_KNOTS('',3,(#26328,#26329,#26330,#26331,#26332,
#26333),.UNSPECIFIED.,.F.,.F.,(4,2,4),(-0.346239220973872,-0.227029016346038,
-9.99999999473644E-7),.UNSPECIFIED.);
#372=B_SPLINE_CURVE_WITH_KNOTS('',3,(#26336,#26337,#26338,#26339,#26340,
#26341,#26342,#26343,#26344,#26345,#26346,#26347,#26348,#26349,#26350,#26351),
 .UNSPECIFIED.,.F.,.F.,(4,3,3,3,3,4),(0.,0.000451322032191559,0.000929732914751349,
0.00118344017626207,0.00236688035252415,0.0047337607050483),
 .UNSPECIFIED.);
#373=B_SPLINE_CURVE_WITH_KNOTS('',3,(#26352,#26353,#26354,#26355,#26356,
#26357,#26358,#26359,#26360,#26361,#26362,#26363,#26364,#26365,#26366,#26367,
#26368,#26369,#26370,#26371,#26372,#26373,#26374,#26375,#26376,#26377,#26378,
#26379,#26380,#26381,#26382,#26383,#26384,#26385,#26386,#26387,#26388,#26389,
#26390,#26391),.UNSPECIFIED.,.F.,.F.,(4,3,3,3,3,3,3,3,3,3,3,3,3,4),(0.,
0.000185189249441203,0.000368062392512153,0.000370402020091198,0.000660760771445963,
0.000736124785024307,0.000740751361344412,0.00110965157437254,0.00147224957004861,
0.00147684472482692,0.00187750418039922,0.00220912636931071,0.00266911044484345,
0.0029444991400972),.UNSPECIFIED.);
#374=B_SPLINE_CURVE_WITH_KNOTS('',3,(#26393,#26394,#26395,#26396,#26397,
#26398,#26399,#26400,#26401,#26402,#26403,#26404,#26405,#26406,#26407,#26408,
#26409,#26410,#26411,#26412,#26413,#26414,#26415,#26416,#26417,#26418,#26419,
#26420,#26421,#26422,#26423,#26424,#26425,#26426,#26427,#26428,#26429,#26430,
#26431,#26432,#26433,#26434,#26435),.UNSPECIFIED.,.F.,.F.,(4,3,3,3,3,3,
3,3,3,3,3,3,3,3,4),(-1.60764784209641E-5,0.000499411850648658,0.000723635622661751,
0.000723642899130192,0.00103927233191355,0.0013403986652088,0.0014632911881516,
0.00146336227668135,0.0018331686514735,0.00220304610996557,0.0022030816542325,
0.00257292357087475,0.00257294134300808,0.00275788190338485,0.00294280103178366),
 .UNSPECIFIED.);
#375=B_SPLINE_CURVE_WITH_KNOTS('',3,(#26436,#26437,#26438,#26439,#26440,
#26441,#26442,#26443,#26444,#26445,#26446,#26447,#26448),.UNSPECIFIED.,
 .F.,.F.,(4,3,3,3,4),(0.,0.00234949256753247,0.00326816604257249,0.00408172543590533,
0.00469898513506494),.UNSPECIFIED.);
#376=B_SPLINE_CURVE_WITH_KNOTS('',3,(#26451,#26452,#26453,#26454,#26455,
#26456,#26457,#26458,#26459,#26460,#26461,#26462,#26463,#26464,#26465,#26466),
 .UNSPECIFIED.,.F.,.F.,(4,3,3,3,3,4),(0.,0.000451322031352851,0.000929732913567863,
0.00118344017626208,0.00236688035252417,0.00473376070504833),
 .UNSPECIFIED.);
#377=B_SPLINE_CURVE_WITH_KNOTS('',3,(#26467,#26468,#26469,#26470,#26471,
#26472,#26473,#26474,#26475,#26476,#26477,#26478,#26479,#26480,#26481,#26482,
#26483,#26484,#26485,#26486,#26487,#26488,#26489,#26490,#26491,#26492,#26493,
#26494,#26495,#26496,#26497,#26498,#26499,#26500,#26501,#26502,#26503),
 .UNSPECIFIED.,.F.,.F.,(4,3,3,3,3,3,3,3,3,3,3,3,4),(0.,0.000186086495974917,
0.000372163572863526,0.000372184889337349,0.000744327145727053,0.000744369778660529,
0.00111655466602905,0.0014886542914541,0.00148873955732231,0.00223298143718115,
0.00223309919665271,0.00286524466138102,0.00297730858290821),
 .UNSPECIFIED.);
#378=B_SPLINE_CURVE_WITH_KNOTS('',3,(#26505,#26506,#26507,#26508,#26509,
#26510,#26511,#26512,#26513,#26514,#26515,#26516,#26517,#26518,#26519,#26520,
#26521,#26522,#26523,#26524,#26525,#26526,#26527,#26528,#26529,#26530,#26531,
#26532,#26533,#26534,#26535,#26536,#26537,#26538,#26539,#26540,#26541,#26542,
#26543,#26544,#26545,#26546,#26547),.UNSPECIFIED.,.F.,.F.,(4,3,3,3,3,3,
3,3,3,3,3,3,3,3,4),(-1.60764784223026E-5,0.000499412098106437,0.000723635622661197,
0.000723642899128064,0.00103927233247834,0.00134039866621365,0.00146329118815029,
0.00146336227667843,0.00183316865147226,0.00220304610996427,0.0022030816542288,
0.00257292357087343,0.00257294134300398,0.00275788190338312,0.00294280103177916),
 .UNSPECIFIED.);
#379=B_SPLINE_CURVE_WITH_KNOTS('',3,(#26548,#26549,#26550,#26551,#26552,
#26553,#26554,#26555,#26556,#26557,#26558,#26559,#26560),.UNSPECIFIED.,
 .F.,.F.,(4,3,3,3,4),(0.,0.002349492567534,0.00326816604266149,0.00408172543673988,
0.004698985135068),.UNSPECIFIED.);
#380=B_SPLINE_CURVE_WITH_KNOTS('',3,(#28354,#28355,#28356,#28357,#28358,
#28359,#28360,#28361,#28362,#28363),.UNSPECIFIED.,.F.,.F.,(4,2,2,2,4),(-1.97874132814648E-5,
0.00222205868858777,0.00278252021405508,0.00334298173952239,0.004463904790457),
 .UNSPECIFIED.);
#381=B_SPLINE_CURVE_WITH_KNOTS('',3,(#28455,#28456,#28457,#28458,#28459,
#28460,#28461,#28462,#28463,#28464,#28465,#28466,#28467,#28468,#28469,#28470,
#28471,#28472,#28473,#28474,#28475,#28476,#28477,#28478,#28479,#28480,#28481,
#28482,#28483,#28484,#28485,#28486,#28487,#28488,#28489,#28490,#28491,#28492,
#28493,#28494,#28495,#28496,#28497,#28498,#28499,#28500,#28501,#28502,#28503),
 .UNSPECIFIED.,.F.,.F.,(4,3,3,3,3,3,3,3,3,3,3,3,3,3,3,3,4),(0.,0.000379018093662348,
0.000744171494405515,0.00108379438629942,0.00140978955393366,0.00173094370171073,
0.00202840150890502,0.0020520978494878,0.00232114678039188,0.00262671080521888,
0.00291522316429607,0.00307814677423169,0.00327435230353986,0.00350085469361757,
0.00372101287058707,0.0039314003020558,0.00410419569897559),
 .UNSPECIFIED.);
#382=B_SPLINE_CURVE_WITH_KNOTS('',3,(#28505,#28506,#28507,#28508,#28509,
#28510,#28511,#28512,#28513,#28514,#28515,#28516,#28517,#28518,#28519,#28520,
#28521,#28522,#28523,#28524,#28525,#28526,#28527,#28528,#28529,#28530,#28531,
#28532,#28533,#28534,#28535,#28536,#28537,#28538,#28539,#28540,#28541,#28542,
#28543,#28544,#28545,#28546,#28547),.UNSPECIFIED.,.F.,.F.,(4,3,3,3,3,3,
3,3,3,3,3,3,3,3,4),(0.,0.000237141843545166,0.00048768786178728,0.000757439823406238,
0.0010271917850252,0.00130827499283397,0.00160260588705221,0.0017756125446872,
0.00205438357005039,0.002361793104946,0.00268278078634015,0.00301878732570562,
0.00337857137823455,0.00376136364485667,0.00410876714010079),
 .UNSPECIFIED.);
#383=B_SPLINE_CURVE_WITH_KNOTS('',3,(#28579,#28580,#28581,#28582,#28583,
#28584,#28585,#28586,#28587,#28588,#28589,#28590),.UNSPECIFIED.,.F.,.F.,
(4,2,2,2,2,4),(9.92648521184955E-17,0.00111453019999537,0.00167179529999301,
0.00222906039999065,0.00334359059998592,0.0044581207999812),
 .UNSPECIFIED.);
#384=B_SPLINE_CURVE_WITH_KNOTS('',3,(#28622,#28623,#28624,#28625,#28626,
#28627,#28628,#28629,#28630,#28631),.UNSPECIFIED.,.F.,.F.,(4,2,2,2,4),(-1.97874132811905E-5,
0.00222205868858802,0.00278252021405532,0.00334298173952263,0.00446390479045723),
 .UNSPECIFIED.);
#385=B_SPLINE_CURVE_WITH_KNOTS('',3,(#28723,#28724,#28725,#28726,#28727,
#28728,#28729,#28730,#28731,#28732,#28733,#28734,#28735,#28736,#28737,#28738,
#28739,#28740,#28741,#28742,#28743,#28744,#28745,#28746,#28747,#28748,#28749,
#28750,#28751,#28752,#28753,#28754,#28755,#28756,#28757,#28758,#28759,#28760,
#28761,#28762,#28763,#28764,#28765,#28766,#28767,#28768,#28769,#28770,#28771),
 .UNSPECIFIED.,.F.,.F.,(4,3,3,3,3,3,3,3,3,3,3,3,3,3,3,3,4),(0.,0.000379018092565528,
0.00074417149243569,0.00108379438364185,0.00140978955067594,0.00173094370008185,
0.0020284015067481,0.00205209784948776,0.0023211467803934,0.00262671080542169,
0.00291522316466974,0.00307814677423164,0.00327435230354241,0.00350085469357018,
0.00372101287049888,0.00393140030193836,0.00410419569897552),
 .UNSPECIFIED.);
#386=B_SPLINE_CURVE_WITH_KNOTS('',3,(#28773,#28774,#28775,#28776,#28777,
#28778,#28779,#28780,#28781,#28782,#28783,#28784,#28785,#28786,#28787,#28788,
#28789,#28790,#28791,#28792,#28793,#28794,#28795,#28796,#28797,#28798,#28799,
#28800,#28801,#28802,#28803,#28804,#28805,#28806,#28807,#28808,#28809,#28810,
#28811,#28812,#28813,#28814,#28815),.UNSPECIFIED.,.F.,.F.,(4,3,3,3,3,3,
3,3,3,3,3,3,3,3,4),(0.,0.000237141844569432,0.000487687864522147,0.000757439824773671,
0.00102719178502519,0.00130827499701704,0.00160260589471355,0.00177561254466418,
0.00205438357005039,0.00236179310188202,0.00268278077972904,0.00301878731501841,
0.00337857136277177,0.00376136362374476,0.00410876714010078),
 .UNSPECIFIED.);
#387=B_SPLINE_CURVE_WITH_KNOTS('',3,(#28847,#28848,#28849,#28850,#28851,
#28852,#28853,#28854,#28855,#28856,#28857,#28858),.UNSPECIFIED.,.F.,.F.,
(4,2,2,2,2,4),(9.56971647899676E-17,0.00111453019999533,0.00167179529999294,
0.00222906039999056,0.00334359059998579,0.00445812079998102),
 .UNSPECIFIED.);
#388=B_SPLINE_CURVE_WITH_KNOTS('',3,(#29368,#29369,#29370,#29371,#29372,
#29373,#29374,#29375),.UNSPECIFIED.,.F.,.F.,(4,2,2,4),(9.99999998608377E-7,
0.266379961876312,0.531813270515335,0.536353198987997),.UNSPECIFIED.);
#389=B_SPLINE_CURVE_WITH_KNOTS('',3,(#29381,#29382,#29383,#29384,#29385,
#29386,#29387,#29388,#29389,#29390,#29391,#29392,#29393,#29394,#29395,#29396,
#29397,#29398,#29399,#29400,#29401,#29402,#29403,#29404,#29405,#29406,#29407,
#29408,#29409,#29410,#29411,#29412,#29413,#29414,#29415,#29416),
 .UNSPECIFIED.,.F.,.F.,(4,2,2,2,2,2,2,2,2,2,2,2,2,2,2,2,2,4),(22.8834714331197,
22.9155217152857,23.2228277353395,23.5358042737047,23.8457116148797,24.1541920344525,
24.4699609353675,24.7777751890622,25.0888369401879,25.401624583911,25.7090811724736,
26.0228085024749,26.332036183219,26.6411952597108,26.9577480048216,27.265398063477,
27.5359657548391,27.8035129251823),.UNSPECIFIED.);
#390=B_SPLINE_CURVE_WITH_KNOTS('',3,(#29418,#29419,#29420,#29421,#29422,
#29423,#29424,#29425,#29426,#29427,#29428,#29429,#29430,#29431,#29432,#29433,
#29434,#29435,#29436,#29437,#29438,#29439,#29440,#29441,#29442,#29443,#29444,
#29445,#29446,#29447,#29448,#29449,#29450,#29451,#29452,#29453),
 .UNSPECIFIED.,.F.,.F.,(4,2,2,2,2,2,2,2,2,2,2,2,2,2,2,2,2,4),(0.536353198987997,
0.844009151960195,1.15538573983787,1.46301980084842,1.7791232671795,2.0878690803984,
2.39732301411271,2.71061683058146,3.01790845407002,3.33114842108659,3.6418042399083,
3.94969512235302,4.26503959484436,4.57319165957025,4.88342264885394,5.19599272714235,
5.50322598252289,5.5439768298363),.UNSPECIFIED.);
#391=B_SPLINE_CURVE_WITH_KNOTS('',3,(#29458,#29459,#29460,#29461,#29462,
#29463,#29464,#29465,#29466,#29467,#29468,#29469,#29470,#29471,#29472,#29473,
#29474,#29475,#29476,#29477,#29478,#29479,#29480,#29481,#29482,#29483,#29484,
#29485,#29486,#29487,#29488,#29489,#29490,#29491,#29492,#29493),
 .UNSPECIFIED.,.F.,.F.,(4,2,2,2,2,2,2,2,2,2,2,2,2,2,2,2,2,4),(17.8745023500825,
17.9426329487553,18.2502173426604,18.5619029033133,18.8737351023357,19.1814304857963,
19.4958276241938,19.8045434042373,20.1142954786953,20.4295794098716,20.7369298255106,
21.0492181265779,21.360004308523,21.6679912272627,21.983034000075,22.2912070574588,
22.601577623486,22.8834714331197),.UNSPECIFIED.);
#392=B_SPLINE_CURVE_WITH_KNOTS('',3,(#29494,#29495,#29496,#29497,#29498,
#29499,#29500,#29501,#29502,#29503,#29504,#29505,#29506,#29507,#29508,#29509,
#29510,#29511,#29512,#29513,#29514,#29515,#29516,#29517,#29518,#29519,#29520,
#29521,#29522,#29523,#29524,#29525,#29526,#29527,#29528,#29529),
 .UNSPECIFIED.,.F.,.F.,(4,2,2,2,2,2,2,2,2,2,2,2,2,2,2,2,2,4),(5.5439768298363,
5.8177146782931,6.12771125014353,6.43605042222614,6.75070419648573,7.05845758227753,
7.36965133741442,7.68157100910749,7.98894019875319,8.30483846765822,8.61425879594142,
8.92321980318127,9.23727438509702,9.54483326301095,9.85713746478567,10.1685030197442,
10.4761899795599,10.5523964499815),.UNSPECIFIED.);
#393=B_SPLINE_CURVE_WITH_KNOTS('',3,(#29534,#29535,#29536,#29537,#29538,
#29539,#29540,#29541,#29542,#29543,#29544,#29545,#29546,#29547,#29548,#29549,
#29550,#29551,#29552,#29553,#29554,#29555,#29556,#29557,#29558,#29559,#29560,
#29561,#29562,#29563,#29564,#29565,#29566,#29567,#29568,#29569),
 .UNSPECIFIED.,.F.,.F.,(4,2,2,2,2,2,2,2,2,2,2,2,2,2,2,2,2,4),(12.8667522473679,
12.9699770959428,13.2778173876454,13.5932720524022,13.9015013605794,14.2087341790668,
14.5215936127585,14.8314800687057,15.1398530720226,15.4555019865385,15.7632628653506,
16.0742081083735,16.3869911773338,16.694362346664,17.0079690989337,17.3171627992321,
17.6262033882063,17.8745023500825),.UNSPECIFIED.);
#394=B_SPLINE_CURVE_WITH_KNOTS('',3,(#29570,#29571,#29572,#29573,#29574,
#29575,#29576,#29577,#29578,#29579,#29580,#29581,#29582,#29583,#29584,#29585,
#29586,#29587,#29588,#29589,#29590,#29591,#29592,#29593,#29594,#29595,#29596,
#29597,#29598,#29599,#29600,#29601,#29602,#29603,#29604,#29605),
 .UNSPECIFIED.,.F.,.F.,(4,2,2,2,2,2,2,2,2,2,2,2,2,2,2,2,2,4),(10.5523964499815,
10.7922801625917,11.1010192151014,11.4105628806873,11.7238453805044,12.0311675378644,
12.344531578361,12.655179957593,12.9631375944165,13.2784727772684,13.5866311789278,
13.8969661452367,14.2099076813701,14.5197896220926,14.8282363019679,15.1439697099529,
15.4517555491791,15.5606140240025),.UNSPECIFIED.);
#395=B_SPLINE_CURVE_WITH_KNOTS('',3,(#29610,#29611,#29612,#29613,#29614,
#29615,#29616,#29617,#29618,#29619,#29620,#29621,#29622,#29623,#29624,#29625,
#29626,#29627,#29628,#29629,#29630,#29631,#29632,#29633,#29634,#29635,#29636,
#29637,#29638,#29639,#29640,#29641,#29642,#29643,#29644,#29645),
 .UNSPECIFIED.,.F.,.F.,(4,2,2,2,2,2,2,2,2,2,2,2,2,2,2,2,2,4),(7.85839646972881,
7.99675908034552,8.30409236965206,8.61967918417833,8.92922883729377,9.23804955367523,
9.55223789637168,9.85983263591087,10.1718920011921,10.4833809125238,10.790993638598,
11.107215596657,11.4160660862887,11.7254216174803,12.0388290447384,12.3461464639337,
12.6592164371347,12.8667522473679),.UNSPECIFIED.);
#396=B_SPLINE_CURVE_WITH_KNOTS('',3,(#29646,#29647,#29648,#29649,#29650,
#29651,#29652,#29653,#29654,#29655,#29656,#29657,#29658,#29659,#29660,#29661,
#29662,#29663,#29664,#29665,#29666,#29667,#29668,#29669,#29670,#29671,#29672,
#29673,#29674,#29675,#29676,#29677,#29678,#29679,#29680,#29681),
 .UNSPECIFIED.,.F.,.F.,(4,2,2,2,2,2,2,2,2,2,2,2,2,2,2,2,2,4),(15.5606140240025,
15.7627825023106,16.0755461176622,16.3829711914898,16.6966631273082,17.005864177191,
17.3149883873622,17.6315052718071,17.9391257290499,18.2508955674803,18.5627214169535,
18.8704807789836,19.1849651185974,19.4937006141905,19.8035378336403,20.118799733417,
20.4261960881153,20.5702181520879),.UNSPECIFIED.);
#397=B_SPLINE_CURVE_WITH_KNOTS('',3,(#29687,#29688,#29689,#29690,#29691,
#29692,#29693,#29694,#29695,#29696,#29697,#29698,#29699,#29700,#29701,#29702,
#29703,#29704),.UNSPECIFIED.,.F.,.F.,(4,2,2,2,2,2,2,2,4),(25.5798166940227,
25.7130762262509,26.0223265959452,26.3315808307711,26.6482322244482,26.9559321724754,
27.2678326511296,27.5344395661045,27.8029491759931),.UNSPECIFIED.);
#398=B_SPLINE_CURVE_WITH_KNOTS('',3,(#29707,#29708,#29709,#29710,#29711,
#29712,#29713,#29714,#29715,#29716,#29717,#29718,#29719,#29720,#29721,#29722,
#29723,#29724,#29725,#29726,#29727,#29728),.UNSPECIFIED.,.F.,.F.,(4,2,2,
2,2,2,2,2,2,2,4),(0.,0.268131059792874,0.538872031707751,0.846503258776113,
1.15851001858798,1.47006242806841,1.77767654293643,2.09396510009836,2.40287638170031,
2.71219706537191,2.85070864589331),.UNSPECIFIED.);
#399=B_SPLINE_CURVE_WITH_KNOTS('',3,(#29749,#29750,#29751,#29752,#29753,
#29754,#29755),.UNSPECIFIED.,.F.,.F.,(4,3,4),(6.13365413464591E-7,0.000387864803977344,
0.000603704646788277),.UNSPECIFIED.);
#400=B_SPLINE_CURVE_WITH_KNOTS('',3,(#29761,#29762,#29763,#29764,#29765,
#29766,#29767),.UNSPECIFIED.,.F.,.F.,(4,3,4),(0.000817437436689343,0.00120468887525266,
0.00142052871806415),.UNSPECIFIED.);
#401=B_SPLINE_CURVE_WITH_KNOTS('',3,(#29772,#29773,#29774,#29775,#29776,
#29777,#29778,#29779,#29780,#29781,#29782,#29783,#29784,#29785,#29786,#29787,
#29788,#29789,#29790,#29791,#29792,#29793,#29794,#29795,#29796,#29797,#29798,
#29799,#29800,#29801,#29802,#29803,#29804,#29805,#29806,#29807),
 .UNSPECIFIED.,.F.,.F.,(4,2,2,2,2,2,2,2,2,2,2,2,2,2,2,2,2,4),(2.85070864589331,
3.02566872683572,3.33300978172351,3.64601116007675,3.95683190204972,4.26465975012339,
4.5801772316469,4.88845455104737,5.19850753800061,5.51124232253364,5.81848197490562,
6.13269024613722,6.44283634473625,6.75107126604603,7.06588097711394,7.37371520837401,
7.68469288372467,7.85839646972881),.UNSPECIFIED.);
#402=B_SPLINE_CURVE_WITH_KNOTS('',3,(#29808,#29809,#29810,#29811,#29812,
#29813,#29814,#29815,#29816,#29817,#29818,#29819,#29820,#29821,#29822,#29823,
#29824,#29825,#29826,#29827,#29828,#29829,#29830,#29831,#29832,#29833,#29834,
#29835,#29836,#29837,#29838,#29839,#29840,#29841,#29842,#29843),
 .UNSPECIFIED.,.F.,.F.,(4,2,2,2,2,2,2,2,2,2,2,2,2,2,2,2,2,4),(20.5702181520879,
20.7385740104812,21.0493617127615,21.3574237984673,21.6725588611289,21.9807610000102,
22.2912213303042,22.6051519312801,22.9125144828566,23.2255847455386,23.5355035868745,
23.8440698995767,24.1599349233628,24.4677886469063,24.7789436195636,25.0917287398098,
25.3992523291087,25.5798166940227),.UNSPECIFIED.);
#403=B_SPLINE_CURVE_WITH_KNOTS('',3,(#29874,#29875,#29876,#29877),
 .UNSPECIFIED.,.F.,.F.,(4,4),(0.0216842181230129,0.0225335408556301),
 .UNSPECIFIED.);
#404=B_SPLINE_CURVE_WITH_KNOTS('',3,(#29915,#29916,#29917,#29918,#29919,
#29920,#29921,#29922,#29923,#29924,#29925,#29926,#29927,#29928,#29929,#29930,
#29931,#29932,#29933,#29934),.UNSPECIFIED.,.F.,.F.,(4,2,2,2,2,2,2,2,2,4),
(-1.25100528979193,-1.12527766599275,-0.967452239770817,-0.849922888806208,
-0.710459887734631,-0.570917050432261,-0.500208813989938,-0.376689447115683,
-0.191154661349975,0.),.UNSPECIFIED.);
#405=B_SPLINE_CURVE_WITH_KNOTS('',3,(#29935,#29936,#29937,#29938,#29939,
#29940,#29941,#29942,#29943,#29944,#29945,#29946,#29947,#29948,#29949,#29950),
 .UNSPECIFIED.,.F.,.F.,(4,2,2,2,2,2,2,4),(-2.40428630272802,-2.08547605103358,
-1.77189968896946,-1.56153084332572,-0.979972531621945,-0.535421503321372,
-0.245999800540891,0.),.UNSPECIFIED.);
#406=B_SPLINE_CURVE_WITH_KNOTS('',3,(#29970,#29971,#29972,#29973,#29974,
#29975,#29976,#29977,#29978,#29979,#29980,#29981,#29982,#29983),
 .UNSPECIFIED.,.F.,.F.,(4,2,2,2,2,2,4),(0.,0.217946805567693,0.483860386593378,
0.854449493561944,1.0785820352923,1.63181551227744,2.25117072670807),
 .UNSPECIFIED.);
#407=B_SPLINE_CURVE_WITH_KNOTS('',3,(#29984,#29985,#29986,#29987,#29988,
#29989,#29990,#29991,#29992,#29993,#29994,#29995,#29996,#29997,#29998,#29999,
#30000,#30001,#30002,#30003),.UNSPECIFIED.,.F.,.F.,(4,2,2,2,2,2,2,2,2,4),
(0.,0.13295682621977,0.26569932246445,0.351005745590642,0.636655227537102,
0.703754608612356,0.957682580022869,1.06961165453364,1.15307337275592,1.38824210628559),
 .UNSPECIFIED.);
#408=(
BOUNDED_CURVE()
B_SPLINE_CURVE(2,(#22731,#22732,#22733),.UNSPECIFIED.,.F.,.F.)
B_SPLINE_CURVE_WITH_KNOTS((3,3),(2.04583671611078,3.4301435642622),
 .UNSPECIFIED.)
CURVE()
GEOMETRIC_REPRESENTATION_ITEM()
RATIONAL_B_SPLINE_CURVE((1.65994685877124,1.78834419513797,1.78834419513797))
REPRESENTATION_ITEM('')
);
#409=(
BOUNDED_CURVE()
B_SPLINE_CURVE(2,(#22740,#22741,#22742),.UNSPECIFIED.,.F.,.F.)
B_SPLINE_CURVE_WITH_KNOTS((3,3),(3.4301435642622,4.81445041241362),
 .UNSPECIFIED.)
CURVE()
GEOMETRIC_REPRESENTATION_ITEM()
RATIONAL_B_SPLINE_CURVE((1.78834419513797,1.78834419513797,1.65994685877124))
REPRESENTATION_ITEM('')
);
#410=(
BOUNDED_CURVE()
B_SPLINE_CURVE(2,(#22746,#22747,#22748),.UNSPECIFIED.,.F.,.F.)
B_SPLINE_CURVE_WITH_KNOTS((3,3),(2.04583671611078,3.4301435642622),
 .UNSPECIFIED.)
CURVE()
GEOMETRIC_REPRESENTATION_ITEM()
RATIONAL_B_SPLINE_CURVE((1.65994685877124,1.78834419513797,1.78834419513797))
REPRESENTATION_ITEM('')
);
#411=(
BOUNDED_CURVE()
B_SPLINE_CURVE(2,(#22752,#22753,#22754),.UNSPECIFIED.,.F.,.F.)
B_SPLINE_CURVE_WITH_KNOTS((3,3),(3.4301435642622,4.81445041241363),
 .UNSPECIFIED.)
CURVE()
GEOMETRIC_REPRESENTATION_ITEM()
RATIONAL_B_SPLINE_CURVE((1.78834419513797,1.78834419513797,1.65994685877124))
REPRESENTATION_ITEM('')
);
#412=(
BOUNDED_CURVE()
B_SPLINE_CURVE(2,(#22758,#22759,#22760),.UNSPECIFIED.,.F.,.F.)
B_SPLINE_CURVE_WITH_KNOTS((3,3),(2.04583671611078,3.4301435642622),
 .UNSPECIFIED.)
CURVE()
GEOMETRIC_REPRESENTATION_ITEM()
RATIONAL_B_SPLINE_CURVE((1.65994685877124,1.78834419513797,1.78834419513797))
REPRESENTATION_ITEM('')
);
#413=(
BOUNDED_CURVE()
B_SPLINE_CURVE(2,(#22764,#22765,#22766),.UNSPECIFIED.,.F.,.F.)
B_SPLINE_CURVE_WITH_KNOTS((3,3),(3.4301435642622,4.81445041241362),
 .UNSPECIFIED.)
CURVE()
GEOMETRIC_REPRESENTATION_ITEM()
RATIONAL_B_SPLINE_CURVE((1.78834419513797,1.78834419513797,1.65994685877124))
REPRESENTATION_ITEM('')
);
#414=(
BOUNDED_CURVE()
B_SPLINE_CURVE(2,(#22770,#22771,#22772),.UNSPECIFIED.,.F.,.F.)
B_SPLINE_CURVE_WITH_KNOTS((3,3),(2.04583671611077,3.4301435642622),
 .UNSPECIFIED.)
CURVE()
GEOMETRIC_REPRESENTATION_ITEM()
RATIONAL_B_SPLINE_CURVE((1.65994685877124,1.78834419513797,1.78834419513797))
REPRESENTATION_ITEM('')
);
#415=(
BOUNDED_CURVE()
B_SPLINE_CURVE(2,(#22776,#22777,#22778),.UNSPECIFIED.,.F.,.F.)
B_SPLINE_CURVE_WITH_KNOTS((3,3),(3.4301435642622,4.81445041241362),
 .UNSPECIFIED.)
CURVE()
GEOMETRIC_REPRESENTATION_ITEM()
RATIONAL_B_SPLINE_CURVE((1.78834419513797,1.78834419513797,1.65994685877124))
REPRESENTATION_ITEM('')
);
#416=(
BOUNDED_CURVE()
B_SPLINE_CURVE(2,(#22782,#22783,#22784),.UNSPECIFIED.,.F.,.F.)
B_SPLINE_CURVE_WITH_KNOTS((3,3),(2.04583671611079,3.4301435642622),
 .UNSPECIFIED.)
CURVE()
GEOMETRIC_REPRESENTATION_ITEM()
RATIONAL_B_SPLINE_CURVE((1.65994685877123,1.78834419513797,1.78834419513797))
REPRESENTATION_ITEM('')
);
#417=(
BOUNDED_CURVE()
B_SPLINE_CURVE(2,(#22788,#22789,#22790),.UNSPECIFIED.,.F.,.F.)
B_SPLINE_CURVE_WITH_KNOTS((3,3),(3.4301435642622,4.81445041241362),
 .UNSPECIFIED.)
CURVE()
GEOMETRIC_REPRESENTATION_ITEM()
RATIONAL_B_SPLINE_CURVE((1.78834419513797,1.78834419513797,1.65994685877123))
REPRESENTATION_ITEM('')
);
#418=(
BOUNDED_CURVE()
B_SPLINE_CURVE(2,(#22793,#22794,#22795),.UNSPECIFIED.,.F.,.F.)
B_SPLINE_CURVE_WITH_KNOTS((3,3),(2.04583671611079,3.4301435642622),
 .UNSPECIFIED.)
CURVE()
GEOMETRIC_REPRESENTATION_ITEM()
RATIONAL_B_SPLINE_CURVE((1.65994685877124,1.78834419513797,1.78834419513797))
REPRESENTATION_ITEM('')
);
#419=(
BOUNDED_CURVE()
B_SPLINE_CURVE(2,(#22797,#22798,#22799),.UNSPECIFIED.,.F.,.F.)
B_SPLINE_CURVE_WITH_KNOTS((3,3),(3.4301435642622,4.81445041241362),
 .UNSPECIFIED.)
CURVE()
GEOMETRIC_REPRESENTATION_ITEM()
RATIONAL_B_SPLINE_CURVE((1.78834419513797,1.78834419513797,1.65994685877124))
REPRESENTATION_ITEM('')
);
#420=(
BOUNDED_CURVE()
B_SPLINE_CURVE(2,(#22829,#22830,#22831),.UNSPECIFIED.,.F.,.F.)
B_SPLINE_CURVE_WITH_KNOTS((3,3),(2.04583671611078,3.43014356426221),
 .UNSPECIFIED.)
CURVE()
GEOMETRIC_REPRESENTATION_ITEM()
RATIONAL_B_SPLINE_CURVE((1.65994685877124,1.78834419513798,1.78834419513798))
REPRESENTATION_ITEM('')
);
#421=(
BOUNDED_CURVE()
B_SPLINE_CURVE(2,(#22838,#22839,#22840),.UNSPECIFIED.,.F.,.F.)
B_SPLINE_CURVE_WITH_KNOTS((3,3),(3.43014356426221,4.81445041241362),
 .UNSPECIFIED.)
CURVE()
GEOMETRIC_REPRESENTATION_ITEM()
RATIONAL_B_SPLINE_CURVE((1.78834419513797,1.78834419513797,1.65994685877124))
REPRESENTATION_ITEM('')
);
#422=(
BOUNDED_CURVE()
B_SPLINE_CURVE(2,(#22844,#22845,#22846),.UNSPECIFIED.,.F.,.F.)
B_SPLINE_CURVE_WITH_KNOTS((3,3),(2.04583671611079,3.4301435642622),
 .UNSPECIFIED.)
CURVE()
GEOMETRIC_REPRESENTATION_ITEM()
RATIONAL_B_SPLINE_CURVE((1.65994685877124,1.78834419513797,1.78834419513797))
REPRESENTATION_ITEM('')
);
#423=(
BOUNDED_CURVE()
B_SPLINE_CURVE(2,(#22850,#22851,#22852),.UNSPECIFIED.,.F.,.F.)
B_SPLINE_CURVE_WITH_KNOTS((3,3),(3.4301435642622,4.81445041241363),
 .UNSPECIFIED.)
CURVE()
GEOMETRIC_REPRESENTATION_ITEM()
RATIONAL_B_SPLINE_CURVE((1.78834419513797,1.78834419513797,1.65994685877124))
REPRESENTATION_ITEM('')
);
#424=(
BOUNDED_CURVE()
B_SPLINE_CURVE(2,(#22856,#22857,#22858),.UNSPECIFIED.,.F.,.F.)
B_SPLINE_CURVE_WITH_KNOTS((3,3),(2.04583671611079,3.43014356426221),
 .UNSPECIFIED.)
CURVE()
GEOMETRIC_REPRESENTATION_ITEM()
RATIONAL_B_SPLINE_CURVE((1.65994685877124,1.78834419513797,1.78834419513797))
REPRESENTATION_ITEM('')
);
#425=(
BOUNDED_CURVE()
B_SPLINE_CURVE(2,(#22862,#22863,#22864),.UNSPECIFIED.,.F.,.F.)
B_SPLINE_CURVE_WITH_KNOTS((3,3),(3.43014356426221,4.81445041241362),
 .UNSPECIFIED.)
CURVE()
GEOMETRIC_REPRESENTATION_ITEM()
RATIONAL_B_SPLINE_CURVE((1.78834419513797,1.78834419513797,1.65994685877124))
REPRESENTATION_ITEM('')
);
#426=(
BOUNDED_CURVE()
B_SPLINE_CURVE(2,(#22868,#22869,#22870),.UNSPECIFIED.,.F.,.F.)
B_SPLINE_CURVE_WITH_KNOTS((3,3),(2.04583671611078,3.4301435642622),
 .UNSPECIFIED.)
CURVE()
GEOMETRIC_REPRESENTATION_ITEM()
RATIONAL_B_SPLINE_CURVE((1.65994685877124,1.78834419513797,1.78834419513797))
REPRESENTATION_ITEM('')
);
#427=(
BOUNDED_CURVE()
B_SPLINE_CURVE(2,(#22874,#22875,#22876),.UNSPECIFIED.,.F.,.F.)
B_SPLINE_CURVE_WITH_KNOTS((3,3),(3.4301435642622,4.81445041241362),
 .UNSPECIFIED.)
CURVE()
GEOMETRIC_REPRESENTATION_ITEM()
RATIONAL_B_SPLINE_CURVE((1.78834419513797,1.78834419513797,1.65994685877124))
REPRESENTATION_ITEM('')
);
#428=(
BOUNDED_CURVE()
B_SPLINE_CURVE(2,(#22880,#22881,#22882),.UNSPECIFIED.,.F.,.F.)
B_SPLINE_CURVE_WITH_KNOTS((3,3),(2.04583671611079,3.4301435642622),
 .UNSPECIFIED.)
CURVE()
GEOMETRIC_REPRESENTATION_ITEM()
RATIONAL_B_SPLINE_CURVE((1.65994685877124,1.78834419513797,1.78834419513797))
REPRESENTATION_ITEM('')
);
#429=(
BOUNDED_CURVE()
B_SPLINE_CURVE(2,(#22886,#22887,#22888),.UNSPECIFIED.,.F.,.F.)
B_SPLINE_CURVE_WITH_KNOTS((3,3),(3.4301435642622,4.81445041241362),
 .UNSPECIFIED.)
CURVE()
GEOMETRIC_REPRESENTATION_ITEM()
RATIONAL_B_SPLINE_CURVE((1.78834419513797,1.78834419513797,1.65994685877124))
REPRESENTATION_ITEM('')
);
#430=(
BOUNDED_CURVE()
B_SPLINE_CURVE(2,(#22891,#22892,#22893),.UNSPECIFIED.,.F.,.F.)
B_SPLINE_CURVE_WITH_KNOTS((3,3),(2.04583671611079,3.4301435642622),
 .UNSPECIFIED.)
CURVE()
GEOMETRIC_REPRESENTATION_ITEM()
RATIONAL_B_SPLINE_CURVE((1.65994685877124,1.78834419513797,1.78834419513797))
REPRESENTATION_ITEM('')
);
#431=(
BOUNDED_CURVE()
B_SPLINE_CURVE(2,(#22895,#22896,#22897),.UNSPECIFIED.,.F.,.F.)
B_SPLINE_CURVE_WITH_KNOTS((3,3),(3.4301435642622,4.81445041241363),
 .UNSPECIFIED.)
CURVE()
GEOMETRIC_REPRESENTATION_ITEM()
RATIONAL_B_SPLINE_CURVE((1.78834419513797,1.78834419513797,1.65994685877124))
REPRESENTATION_ITEM('')
);
#432=(
BOUNDED_CURVE()
B_SPLINE_CURVE(2,(#22941,#22942,#22943),.UNSPECIFIED.,.F.,.F.)
B_SPLINE_CURVE_WITH_KNOTS((3,3),(1.8281284674419,3.10267439666174),
 .UNSPECIFIED.)
CURVE()
GEOMETRIC_REPRESENTATION_ITEM()
RATIONAL_B_SPLINE_CURVE((1.61557985032884,1.7405453866491,1.7405453866491))
REPRESENTATION_ITEM('')
);
#433=(
BOUNDED_CURVE()
B_SPLINE_CURVE(2,(#22945,#22946,#22947),.UNSPECIFIED.,.F.,.F.)
B_SPLINE_CURVE_WITH_KNOTS((3,3),(3.10267439666174,4.3772203258816),
 .UNSPECIFIED.)
CURVE()
GEOMETRIC_REPRESENTATION_ITEM()
RATIONAL_B_SPLINE_CURVE((1.7405453866491,1.7405453866491,1.61557985032884))
REPRESENTATION_ITEM('')
);
#434=(
BOUNDED_CURVE()
B_SPLINE_CURVE(2,(#22951,#22952,#22953),.UNSPECIFIED.,.F.,.F.)
B_SPLINE_CURVE_WITH_KNOTS((3,3),(-3.10267439666174,-1.82812846744189),
 .UNSPECIFIED.)
CURVE()
GEOMETRIC_REPRESENTATION_ITEM()
RATIONAL_B_SPLINE_CURVE((1.74054538664911,1.74054538664911,1.61557985032884))
REPRESENTATION_ITEM('')
);
#435=(
BOUNDED_CURVE()
B_SPLINE_CURVE(2,(#22954,#22955,#22956),.UNSPECIFIED.,.F.,.F.)
B_SPLINE_CURVE_WITH_KNOTS((3,3),(-4.37722032588159,-3.10267439666174),
 .UNSPECIFIED.)
CURVE()
GEOMETRIC_REPRESENTATION_ITEM()
RATIONAL_B_SPLINE_CURVE((1.61557985032884,1.74054538664911,1.74054538664911))
REPRESENTATION_ITEM('')
);
#436=(
BOUNDED_CURVE()
B_SPLINE_CURVE(2,(#22959,#22960,#22961),.UNSPECIFIED.,.F.,.F.)
B_SPLINE_CURVE_WITH_KNOTS((3,3),(1.82812846744189,3.10267439666174),
 .UNSPECIFIED.)
CURVE()
GEOMETRIC_REPRESENTATION_ITEM()
RATIONAL_B_SPLINE_CURVE((1.61557985032883,1.7405453866491,1.7405453866491))
REPRESENTATION_ITEM('')
);
#437=(
BOUNDED_CURVE()
B_SPLINE_CURVE(2,(#22963,#22964,#22965),.UNSPECIFIED.,.F.,.F.)
B_SPLINE_CURVE_WITH_KNOTS((3,3),(3.10267439666174,4.37722032588159),
 .UNSPECIFIED.)
CURVE()
GEOMETRIC_REPRESENTATION_ITEM()
RATIONAL_B_SPLINE_CURVE((1.7405453866491,1.7405453866491,1.61557985032884))
REPRESENTATION_ITEM('')
);
#438=(
BOUNDED_CURVE()
B_SPLINE_CURVE(2,(#22969,#22970,#22971),.UNSPECIFIED.,.F.,.F.)
B_SPLINE_CURVE_WITH_KNOTS((3,3),(-3.10267439666174,-1.8281284674419),
 .UNSPECIFIED.)
CURVE()
GEOMETRIC_REPRESENTATION_ITEM()
RATIONAL_B_SPLINE_CURVE((1.7405453866491,1.7405453866491,1.61557985032884))
REPRESENTATION_ITEM('')
);
#439=(
BOUNDED_CURVE()
B_SPLINE_CURVE(2,(#22972,#22973,#22974),.UNSPECIFIED.,.F.,.F.)
B_SPLINE_CURVE_WITH_KNOTS((3,3),(-4.37722032588159,-3.10267439666174),
 .UNSPECIFIED.)
CURVE()
GEOMETRIC_REPRESENTATION_ITEM()
RATIONAL_B_SPLINE_CURVE((1.61557985032883,1.7405453866491,1.7405453866491))
REPRESENTATION_ITEM('')
);
#440=(
BOUNDED_CURVE()
B_SPLINE_CURVE(2,(#22978,#22979,#22980),.UNSPECIFIED.,.F.,.F.)
B_SPLINE_CURVE_WITH_KNOTS((3,3),(1.82812846744189,3.10267439666174),
 .UNSPECIFIED.)
CURVE()
GEOMETRIC_REPRESENTATION_ITEM()
RATIONAL_B_SPLINE_CURVE((1.61557985032884,1.7405453866491,1.7405453866491))
REPRESENTATION_ITEM('')
);
#441=(
BOUNDED_CURVE()
B_SPLINE_CURVE(2,(#22984,#22985,#22986),.UNSPECIFIED.,.F.,.F.)
B_SPLINE_CURVE_WITH_KNOTS((3,3),(-4.3772203258816,-3.10267439666174),
 .UNSPECIFIED.)
CURVE()
GEOMETRIC_REPRESENTATION_ITEM()
RATIONAL_B_SPLINE_CURVE((1.61557985032884,1.74054538664911,1.74054538664911))
REPRESENTATION_ITEM('')
);
#442=(
BOUNDED_CURVE()
B_SPLINE_CURVE(2,(#22987,#22988,#22989),.UNSPECIFIED.,.F.,.F.)
B_SPLINE_CURVE_WITH_KNOTS((3,3),(-3.10267439666174,-1.82812846744189),
 .UNSPECIFIED.)
CURVE()
GEOMETRIC_REPRESENTATION_ITEM()
RATIONAL_B_SPLINE_CURVE((1.74054538664911,1.74054538664911,1.61557985032884))
REPRESENTATION_ITEM('')
);
#443=(
BOUNDED_CURVE()
B_SPLINE_CURVE(2,(#22990,#22991,#22992),.UNSPECIFIED.,.F.,.F.)
B_SPLINE_CURVE_WITH_KNOTS((3,3),(3.10267439666174,4.3772203258816),
 .UNSPECIFIED.)
CURVE()
GEOMETRIC_REPRESENTATION_ITEM()
RATIONAL_B_SPLINE_CURVE((1.7405453866491,1.7405453866491,1.61557985032884))
REPRESENTATION_ITEM('')
);
#444=(
BOUNDED_CURVE()
B_SPLINE_CURVE(2,(#22995,#22996,#22997),.UNSPECIFIED.,.F.,.F.)
B_SPLINE_CURVE_WITH_KNOTS((3,3),(1.8281284674419,3.10267439666174),
 .UNSPECIFIED.)
CURVE()
GEOMETRIC_REPRESENTATION_ITEM()
RATIONAL_B_SPLINE_CURVE((1.61557985032884,1.7405453866491,1.7405453866491))
REPRESENTATION_ITEM('')
);
#445=(
BOUNDED_CURVE()
B_SPLINE_CURVE(2,(#22999,#23000,#23001),.UNSPECIFIED.,.F.,.F.)
B_SPLINE_CURVE_WITH_KNOTS((3,3),(3.10267439666174,4.3772203258816),
 .UNSPECIFIED.)
CURVE()
GEOMETRIC_REPRESENTATION_ITEM()
RATIONAL_B_SPLINE_CURVE((1.7405453866491,1.7405453866491,1.61557985032883))
REPRESENTATION_ITEM('')
);
#446=(
BOUNDED_CURVE()
B_SPLINE_CURVE(2,(#23005,#23006,#23007),.UNSPECIFIED.,.F.,.F.)
B_SPLINE_CURVE_WITH_KNOTS((3,3),(-3.10267439666174,-1.82812846744189),
 .UNSPECIFIED.)
CURVE()
GEOMETRIC_REPRESENTATION_ITEM()
RATIONAL_B_SPLINE_CURVE((1.7405453866491,1.7405453866491,1.61557985032883))
REPRESENTATION_ITEM('')
);
#447=(
BOUNDED_CURVE()
B_SPLINE_CURVE(2,(#23008,#23009,#23010),.UNSPECIFIED.,.F.,.F.)
B_SPLINE_CURVE_WITH_KNOTS((3,3),(-4.37722032588158,-3.10267439666174),
 .UNSPECIFIED.)
CURVE()
GEOMETRIC_REPRESENTATION_ITEM()
RATIONAL_B_SPLINE_CURVE((1.61557985032883,1.7405453866491,1.7405453866491))
REPRESENTATION_ITEM('')
);
#448=(
BOUNDED_CURVE()
B_SPLINE_CURVE(2,(#23013,#23014,#23015),.UNSPECIFIED.,.F.,.F.)
B_SPLINE_CURVE_WITH_KNOTS((3,3),(1.8281284674419,3.10267439666175),
 .UNSPECIFIED.)
CURVE()
GEOMETRIC_REPRESENTATION_ITEM()
RATIONAL_B_SPLINE_CURVE((1.61557985032884,1.7405453866491,1.7405453866491))
REPRESENTATION_ITEM('')
);
#449=(
BOUNDED_CURVE()
B_SPLINE_CURVE(2,(#23017,#23018,#23019),.UNSPECIFIED.,.F.,.F.)
B_SPLINE_CURVE_WITH_KNOTS((3,3),(3.10267439666175,4.37722032588158),
 .UNSPECIFIED.)
CURVE()
GEOMETRIC_REPRESENTATION_ITEM()
RATIONAL_B_SPLINE_CURVE((1.7405453866491,1.7405453866491,1.61557985032883))
REPRESENTATION_ITEM('')
);
#450=(
BOUNDED_CURVE()
B_SPLINE_CURVE(2,(#23023,#23024,#23025),.UNSPECIFIED.,.F.,.F.)
B_SPLINE_CURVE_WITH_KNOTS((3,3),(-3.10267439666174,-1.8281284674419),
 .UNSPECIFIED.)
CURVE()
GEOMETRIC_REPRESENTATION_ITEM()
RATIONAL_B_SPLINE_CURVE((1.7405453866491,1.7405453866491,1.61557985032884))
REPRESENTATION_ITEM('')
);
#451=(
BOUNDED_CURVE()
B_SPLINE_CURVE(2,(#23026,#23027,#23028),.UNSPECIFIED.,.F.,.F.)
B_SPLINE_CURVE_WITH_KNOTS((3,3),(-4.37722032588158,-3.10267439666174),
 .UNSPECIFIED.)
CURVE()
GEOMETRIC_REPRESENTATION_ITEM()
RATIONAL_B_SPLINE_CURVE((1.61557985032884,1.7405453866491,1.7405453866491))
REPRESENTATION_ITEM('')
);
#452=(
BOUNDED_CURVE()
B_SPLINE_CURVE(2,(#23031,#23032,#23033),.UNSPECIFIED.,.F.,.F.)
B_SPLINE_CURVE_WITH_KNOTS((3,3),(1.82812846744189,3.10267439666174),
 .UNSPECIFIED.)
CURVE()
GEOMETRIC_REPRESENTATION_ITEM()
RATIONAL_B_SPLINE_CURVE((1.61557985032884,1.74054538664911,1.7405453866491))
REPRESENTATION_ITEM('')
);
#453=(
BOUNDED_CURVE()
B_SPLINE_CURVE(2,(#23034,#23035,#23036),.UNSPECIFIED.,.F.,.F.)
B_SPLINE_CURVE_WITH_KNOTS((3,3),(3.10267439666174,4.37722032588159),
 .UNSPECIFIED.)
CURVE()
GEOMETRIC_REPRESENTATION_ITEM()
RATIONAL_B_SPLINE_CURVE((1.74054538664911,1.74054538664911,1.61557985032884))
REPRESENTATION_ITEM('')
);
#454=(
BOUNDED_CURVE()
B_SPLINE_CURVE(2,(#23038,#23039,#23040),.UNSPECIFIED.,.F.,.F.)
B_SPLINE_CURVE_WITH_KNOTS((3,3),(-3.10267439666174,-1.82812846744189),
 .UNSPECIFIED.)
CURVE()
GEOMETRIC_REPRESENTATION_ITEM()
RATIONAL_B_SPLINE_CURVE((1.74054538664911,1.74054538664911,1.61557985032884))
REPRESENTATION_ITEM('')
);
#455=(
BOUNDED_CURVE()
B_SPLINE_CURVE(2,(#23041,#23042,#23043),.UNSPECIFIED.,.F.,.F.)
B_SPLINE_CURVE_WITH_KNOTS((3,3),(-4.3772203258816,-3.10267439666174),
 .UNSPECIFIED.)
CURVE()
GEOMETRIC_REPRESENTATION_ITEM()
RATIONAL_B_SPLINE_CURVE((1.61557985032884,1.74054538664911,1.74054538664911))
REPRESENTATION_ITEM('')
);
#456=(
BOUNDED_CURVE()
B_SPLINE_CURVE(2,(#23076,#23077,#23078,#23079,#23080,#23081,#23082,#23083,
#23084,#23085,#23086),.UNSPECIFIED.,.F.,.F.)
B_SPLINE_CURVE_WITH_KNOTS((3,2,2,2,2,3),(0.00349366271704399,0.00454545454545455,
0.00909090909090909,0.0136363636363636,0.0181818181818182,0.0227272727272727),
 .UNSPECIFIED.)
CURVE()
GEOMETRIC_REPRESENTATION_ITEM()
RATIONAL_B_SPLINE_CURVE((0.982590712260093,0.988674761632765,1.,0.951056516295154,
1.,0.951056516295154,1.,0.951056516295154,1.,0.951056516295154,1.))
REPRESENTATION_ITEM('')
);
#457=(
BOUNDED_CURVE()
B_SPLINE_CURVE(2,(#23089,#23090,#23091,#23092,#23093),.UNSPECIFIED.,.F.,
 .F.)
B_SPLINE_CURVE_WITH_KNOTS((3,2,3),(0.0151375700072014,0.0184727520515342,
0.0230909400644179),.UNSPECIFIED.)
CURVE()
GEOMETRIC_REPRESENTATION_ITEM()
RATIONAL_B_SPLINE_CURVE((0.980360524940442,0.964653793309387,1.,0.951056516295154,
1.))
REPRESENTATION_ITEM('')
);
#458=(
BOUNDED_CURVE()
B_SPLINE_CURVE(2,(#23098,#23099,#23100,#23101,#23102,#23103,#23104,#23105,
#23106,#23107,#23108,#23109,#23110,#23111,#23112,#23113,#23114,#23115,#23116,
#23117,#23118),.UNSPECIFIED.,.F.,.F.)
B_SPLINE_CURVE_WITH_KNOTS((3,2,2,2,2,2,2,2,2,2,3),(0.0227272727272727,0.0272727272727273,
0.0318181818181818,0.0363636363636364,0.0409090909090909,0.0454545454545455,
0.05,0.0545454545454545,0.0590909090909091,0.0636363636363636,0.0681818181818182),
 .UNSPECIFIED.)
CURVE()
GEOMETRIC_REPRESENTATION_ITEM()
RATIONAL_B_SPLINE_CURVE((1.,0.951056516295154,1.,0.951056516295154,1.,0.951056516295154,
1.,0.951056516295154,1.,0.951056516295154,1.,0.951056516295154,1.,0.951056516295154,
1.,0.951056516295154,1.,0.951056516295154,1.,0.951056516295154,1.))
REPRESENTATION_ITEM('')
);
#459=(
BOUNDED_CURVE()
B_SPLINE_CURVE(2,(#23119,#23120,#23121,#23122,#23123,#23124,#23125,#23126,
#23127,#23128,#23129,#23130,#23131,#23132,#23133,#23134,#23135,#23136,#23137,
#23138,#23139),.UNSPECIFIED.,.F.,.F.)
B_SPLINE_CURVE_WITH_KNOTS((3,2,2,2,2,2,2,2,2,2,3),(0.0230909400644179,0.0277091280773016,
0.0323273160901852,0.0369455041030689,0.0415636921159526,0.0461818801288363,
0.05080006814172,0.0554182561546037,0.0600364441674874,0.0646546321803711,
0.0692728201932548),.UNSPECIFIED.)
CURVE()
GEOMETRIC_REPRESENTATION_ITEM()
RATIONAL_B_SPLINE_CURVE((1.,0.951056516295154,1.,0.951056516295154,1.,0.951056516295154,
1.,0.951056516295154,1.,0.951056516295154,1.,0.951056516295154,1.,0.951056516295154,
1.,0.951056516295154,1.,0.951056516295154,1.,0.951056516295154,1.))
REPRESENTATION_ITEM('')
);
#460=(
BOUNDED_CURVE()
B_SPLINE_CURVE(2,(#23144,#23145,#23146,#23147,#23148,#23149,#23150,#23151,
#23152,#23153,#23154,#23155,#23156,#23157,#23158,#23159,#23160,#23161,#23162,
#23163,#23164),.UNSPECIFIED.,.F.,.F.)
B_SPLINE_CURVE_WITH_KNOTS((3,2,2,2,2,2,2,2,2,2,3),(0.0681818181818182,0.0727272727272727,
0.0772727272727273,0.0818181818181818,0.0863636363636364,0.0909090909090909,
0.0954545454545455,0.1,0.104545454545455,0.109090909090909,0.113636363636364),
 .UNSPECIFIED.)
CURVE()
GEOMETRIC_REPRESENTATION_ITEM()
RATIONAL_B_SPLINE_CURVE((1.,0.951056516295154,1.,0.951056516295154,1.,0.951056516295154,
1.,0.951056516295154,1.,0.951056516295154,1.,0.951056516295154,1.,0.951056516295154,
1.,0.951056516295154,1.,0.951056516295154,1.,0.951056516295154,1.))
REPRESENTATION_ITEM('')
);
#461=(
BOUNDED_CURVE()
B_SPLINE_CURVE(2,(#23165,#23166,#23167,#23168,#23169,#23170,#23171,#23172,
#23173,#23174,#23175,#23176,#23177,#23178,#23179,#23180,#23181,#23182,#23183,
#23184,#23185),.UNSPECIFIED.,.F.,.F.)
B_SPLINE_CURVE_WITH_KNOTS((3,2,2,2,2,2,2,2,2,2,3),(0.0692728201932548,0.0738910082061384,
0.0785091962190222,0.0831273842319059,0.0877455722447895,0.0923637602576732,
0.0969819482705569,0.101600136283441,0.106218324296324,0.110836512309208,
0.115454700322092),.UNSPECIFIED.)
CURVE()
GEOMETRIC_REPRESENTATION_ITEM()
RATIONAL_B_SPLINE_CURVE((1.,0.951056516295154,1.,0.951056516295154,1.,0.951056516295154,
1.,0.951056516295154,1.,0.951056516295154,1.,0.951056516295154,1.,0.951056516295154,
1.,0.951056516295154,1.,0.951056516295154,1.,0.951056516295154,1.))
REPRESENTATION_ITEM('')
);
#462=(
BOUNDED_CURVE()
B_SPLINE_CURVE(2,(#23190,#23191,#23192,#23193,#23194,#23195,#23196,#23197,
#23198,#23199,#23200,#23201,#23202,#23203,#23204,#23205,#23206,#23207,#23208,
#23209,#23210),.UNSPECIFIED.,.F.,.F.)
B_SPLINE_CURVE_WITH_KNOTS((3,2,2,2,2,2,2,2,2,2,3),(0.113636363636364,0.118181818181818,
0.122727272727273,0.127272727272727,0.131818181818182,0.136363636363636,
0.140909090909091,0.145454545454545,0.15,0.154545454545455,0.159090909090909),
 .UNSPECIFIED.)
CURVE()
GEOMETRIC_REPRESENTATION_ITEM()
RATIONAL_B_SPLINE_CURVE((1.,0.951056516295154,1.,0.951056516295154,1.,0.951056516295154,
1.,0.951056516295154,1.,0.951056516295154,1.,0.951056516295154,1.,0.951056516295154,
1.,0.951056516295154,1.,0.951056516295154,1.,0.951056516295154,1.))
REPRESENTATION_ITEM('')
);
#463=(
BOUNDED_CURVE()
B_SPLINE_CURVE(2,(#23211,#23212,#23213,#23214,#23215,#23216,#23217,#23218,
#23219,#23220,#23221,#23222,#23223,#23224,#23225,#23226,#23227,#23228,#23229,
#23230,#23231),.UNSPECIFIED.,.F.,.F.)
B_SPLINE_CURVE_WITH_KNOTS((3,2,2,2,2,2,2,2,2,2,3),(0.115454700322092,0.120072888334975,
0.124691076347859,0.129309264360743,0.133927452373626,0.13854564038651,
0.143163828399394,0.147782016412278,0.152400204425161,0.157018392438045,
0.161636580450929),.UNSPECIFIED.)
CURVE()
GEOMETRIC_REPRESENTATION_ITEM()
RATIONAL_B_SPLINE_CURVE((1.,0.951056516295154,1.,0.951056516295154,1.,0.951056516295154,
1.,0.951056516295154,1.,0.951056516295154,1.,0.951056516295154,1.,0.951056516295154,
1.,0.951056516295154,1.,0.951056516295154,1.,0.951056516295154,1.))
REPRESENTATION_ITEM('')
);
#464=(
BOUNDED_CURVE()
B_SPLINE_CURVE(2,(#23236,#23237,#23238,#23239,#23240,#23241,#23242,#23243,
#23244,#23245,#23246,#23247,#23248,#23249,#23250,#23251,#23252,#23253,#23254,
#23255,#23256),.UNSPECIFIED.,.F.,.F.)
B_SPLINE_CURVE_WITH_KNOTS((3,2,2,2,2,2,2,2,2,2,3),(0.159090909090909,0.163636363636364,
0.168181818181818,0.172727272727273,0.177272727272727,0.181818181818182,
0.186363636363636,0.190909090909091,0.195454545454545,0.2,0.204545454545455),
 .UNSPECIFIED.)
CURVE()
GEOMETRIC_REPRESENTATION_ITEM()
RATIONAL_B_SPLINE_CURVE((1.,0.951056516295154,1.,0.951056516295154,1.,0.951056516295154,
1.,0.951056516295154,1.,0.951056516295154,1.,0.951056516295154,1.,0.951056516295154,
1.,0.951056516295154,1.,0.951056516295154,1.,0.951056516295154,1.))
REPRESENTATION_ITEM('')
);
#465=(
BOUNDED_CURVE()
B_SPLINE_CURVE(2,(#23257,#23258,#23259,#23260,#23261,#23262,#23263,#23264,
#23265,#23266,#23267,#23268,#23269,#23270,#23271,#23272,#23273,#23274,#23275,
#23276,#23277),.UNSPECIFIED.,.F.,.F.)
B_SPLINE_CURVE_WITH_KNOTS((3,2,2,2,2,2,2,2,2,2,3),(0.161636580450929,0.166254768463812,
0.170872956476696,0.17549114448958,0.180109332502463,0.184727520515347,
0.189345708528231,0.193963896541114,0.198582084553998,0.203200272566882,
0.207818460579765),.UNSPECIFIED.)
CURVE()
GEOMETRIC_REPRESENTATION_ITEM()
RATIONAL_B_SPLINE_CURVE((1.,0.951056516295154,1.,0.951056516295154,1.,0.951056516295154,
1.,0.951056516295154,1.,0.951056516295154,1.,0.951056516295154,1.,0.951056516295154,
1.,0.951056516295154,1.,0.951056516295154,1.,0.951056516295154,1.))
REPRESENTATION_ITEM('')
);
#466=(
BOUNDED_CURVE()
B_SPLINE_CURVE(2,(#23282,#23283,#23284,#23285,#23286,#23287,#23288,#23289,
#23290,#23291,#23292,#23293,#23294,#23295,#23296,#23297,#23298,#23299,#23300,
#23301,#23302),.UNSPECIFIED.,.F.,.F.)
B_SPLINE_CURVE_WITH_KNOTS((3,2,2,2,2,2,2,2,2,2,3),(0.204545454545455,0.209090909090909,
0.213636363636364,0.218181818181818,0.222727272727273,0.227272727272727,
0.231818181818182,0.236363636363636,0.240909090909091,0.245454545454545,
0.25),.UNSPECIFIED.)
CURVE()
GEOMETRIC_REPRESENTATION_ITEM()
RATIONAL_B_SPLINE_CURVE((1.,0.951056516295154,1.,0.951056516295154,1.,0.951056516295154,
1.,0.951056516295154,1.,0.951056516295154,1.,0.951056516295154,1.,0.951056516295154,
1.,0.951056516295154,1.,0.951056516295154,1.,0.951056516295154,1.))
REPRESENTATION_ITEM('')
);
#467=(
BOUNDED_CURVE()
B_SPLINE_CURVE(2,(#23303,#23304,#23305,#23306,#23307,#23308,#23309,#23310,
#23311,#23312,#23313,#23314,#23315,#23316,#23317,#23318,#23319,#23320,#23321,
#23322,#23323),.UNSPECIFIED.,.F.,.F.)
B_SPLINE_CURVE_WITH_KNOTS((3,2,2,2,2,2,2,2,2,2,3),(0.207818460579765,0.212436648592649,
0.217054836605533,0.221673024618417,0.2262912126313,0.230909400644184,0.235527588657068,
0.240145776669951,0.244763964682835,0.249382152695719,0.254000340708602),
 .UNSPECIFIED.)
CURVE()
GEOMETRIC_REPRESENTATION_ITEM()
RATIONAL_B_SPLINE_CURVE((1.,0.951056516295154,1.,0.951056516295154,1.,0.951056516295154,
1.,0.951056516295154,1.,0.951056516295154,1.,0.951056516295154,1.,0.951056516295154,
1.,0.951056516295154,1.,0.951056516295154,1.,0.951056516295154,1.))
REPRESENTATION_ITEM('')
);
#468=(
BOUNDED_CURVE()
B_SPLINE_CURVE(2,(#23328,#23329,#23330,#23331,#23332,#23333,#23334,#23335,
#23336,#23337,#23338,#23339,#23340,#23341,#23342,#23343,#23344,#23345,#23346,
#23347,#23348),.UNSPECIFIED.,.F.,.F.)
B_SPLINE_CURVE_WITH_KNOTS((3,2,2,2,2,2,2,2,2,2,3),(0.25,0.254545454545455,
0.259090909090909,0.263636363636364,0.268181818181818,0.272727272727273,
0.277272727272727,0.281818181818182,0.286363636363636,0.290909090909091,
0.295454545454545),.UNSPECIFIED.)
CURVE()
GEOMETRIC_REPRESENTATION_ITEM()
RATIONAL_B_SPLINE_CURVE((1.,0.951056516295154,1.,0.951056516295154,1.,0.951056516295154,
1.,0.951056516295154,1.,0.951056516295154,1.,0.951056516295154,1.,0.951056516295154,
1.,0.951056516295154,1.,0.951056516295154,1.,0.951056516295154,1.))
REPRESENTATION_ITEM('')
);
#469=(
BOUNDED_CURVE()
B_SPLINE_CURVE(2,(#23349,#23350,#23351,#23352,#23353,#23354,#23355,#23356,
#23357,#23358,#23359,#23360,#23361,#23362,#23363,#23364,#23365,#23366,#23367,
#23368,#23369),.UNSPECIFIED.,.F.,.F.)
B_SPLINE_CURVE_WITH_KNOTS((3,2,2,2,2,2,2,2,2,2,3),(0.254000340708602,0.258618528721486,
0.26323671673437,0.267854904747253,0.272473092760137,0.277091280773021,
0.281709468785904,0.286327656798788,0.290945844811672,0.295564032824556,
0.300182220837439),.UNSPECIFIED.)
CURVE()
GEOMETRIC_REPRESENTATION_ITEM()
RATIONAL_B_SPLINE_CURVE((1.,0.951056516295154,1.,0.951056516295154,1.,0.951056516295154,
1.,0.951056516295154,1.,0.951056516295154,1.,0.951056516295154,1.,0.951056516295154,
1.,0.951056516295154,1.,0.951056516295154,1.,0.951056516295154,1.))
REPRESENTATION_ITEM('')
);
#470=(
BOUNDED_CURVE()
B_SPLINE_CURVE(2,(#23374,#23375,#23376,#23377,#23378,#23379,#23380,#23381,
#23382,#23383,#23384,#23385,#23386,#23387,#23388,#23389,#23390,#23391,#23392,
#23393,#23394),.UNSPECIFIED.,.F.,.F.)
B_SPLINE_CURVE_WITH_KNOTS((3,2,2,2,2,2,2,2,2,2,3),(0.295454545454545,0.3,
0.304545454545455,0.309090909090909,0.313636363636364,0.318181818181818,
0.322727272727273,0.327272727272727,0.331818181818182,0.336363636363636,
0.340909090909091),.UNSPECIFIED.)
CURVE()
GEOMETRIC_REPRESENTATION_ITEM()
RATIONAL_B_SPLINE_CURVE((1.,0.951056516295154,1.,0.951056516295154,1.,0.951056516295154,
1.,0.951056516295154,1.,0.951056516295154,1.,0.951056516295154,1.,0.951056516295154,
1.,0.951056516295154,1.,0.951056516295154,1.,0.951056516295154,1.))
REPRESENTATION_ITEM('')
);
#471=(
BOUNDED_CURVE()
B_SPLINE_CURVE(2,(#23395,#23396,#23397,#23398,#23399,#23400,#23401,#23402,
#23403,#23404,#23405,#23406,#23407,#23408,#23409,#23410,#23411,#23412,#23413,
#23414,#23415),.UNSPECIFIED.,.F.,.F.)
B_SPLINE_CURVE_WITH_KNOTS((3,2,2,2,2,2,2,2,2,2,3),(0.300182220837439,0.304800408850323,
0.309418596863207,0.31403678487609,0.318654972888974,0.323273160901858,
0.327891348914741,0.332509536927625,0.337127724940509,0.341745912953392,
0.346364100966276),.UNSPECIFIED.)
CURVE()
GEOMETRIC_REPRESENTATION_ITEM()
RATIONAL_B_SPLINE_CURVE((1.,0.951056516295154,1.,0.951056516295154,1.,0.951056516295154,
1.,0.951056516295154,1.,0.951056516295154,1.,0.951056516295154,1.,0.951056516295154,
1.,0.951056516295154,1.,0.951056516295154,1.,0.951056516295154,1.))
REPRESENTATION_ITEM('')
);
#472=(
BOUNDED_CURVE()
B_SPLINE_CURVE(2,(#23420,#23421,#23422,#23423,#23424,#23425,#23426,#23427,
#23428,#23429,#23430,#23431,#23432,#23433,#23434,#23435,#23436,#23437,#23438,
#23439,#23440),.UNSPECIFIED.,.F.,.F.)
B_SPLINE_CURVE_WITH_KNOTS((3,2,2,2,2,2,2,2,2,2,3),(0.340909090909091,0.345454545454546,
0.35,0.354545454545455,0.359090909090909,0.363636363636364,0.368181818181818,
0.372727272727273,0.377272727272727,0.381818181818182,0.386363636363636),
 .UNSPECIFIED.)
CURVE()
GEOMETRIC_REPRESENTATION_ITEM()
RATIONAL_B_SPLINE_CURVE((1.,0.951056516295154,1.,0.951056516295154,1.,0.951056516295154,
1.,0.951056516295154,1.,0.951056516295154,1.,0.951056516295154,1.,0.951056516295154,
1.,0.951056516295154,1.,0.951056516295154,1.,0.951056516295154,1.))
REPRESENTATION_ITEM('')
);
#473=(
BOUNDED_CURVE()
B_SPLINE_CURVE(2,(#23441,#23442,#23443,#23444,#23445,#23446,#23447,#23448,
#23449,#23450,#23451,#23452,#23453,#23454,#23455,#23456,#23457,#23458,#23459,
#23460,#23461),.UNSPECIFIED.,.F.,.F.)
B_SPLINE_CURVE_WITH_KNOTS((3,2,2,2,2,2,2,2,2,2,3),(0.346364100966276,0.35098228897916,
0.355600476992044,0.360218665004927,0.364836853017811,0.369455041030695,
0.374073229043578,0.378691417056462,0.383309605069346,0.387927793082229,
0.392545981095113),.UNSPECIFIED.)
CURVE()
GEOMETRIC_REPRESENTATION_ITEM()
RATIONAL_B_SPLINE_CURVE((1.,0.951056516295154,1.,0.951056516295154,1.,0.951056516295154,
1.,0.951056516295154,1.,0.951056516295154,1.,0.951056516295154,1.,0.951056516295154,
1.,0.951056516295154,1.,0.951056516295154,1.,0.951056516295154,1.))
REPRESENTATION_ITEM('')
);
#474=(
BOUNDED_CURVE()
B_SPLINE_CURVE(2,(#23466,#23467,#23468,#23469,#23470,#23471,#23472,#23473,
#23474,#23475,#23476,#23477,#23478,#23479,#23480,#23481,#23482,#23483,#23484,
#23485,#23486),.UNSPECIFIED.,.F.,.F.)
B_SPLINE_CURVE_WITH_KNOTS((3,2,2,2,2,2,2,2,2,2,3),(0.386363636363636,0.390909090909091,
0.395454545454545,0.4,0.404545454545455,0.409090909090909,0.413636363636364,
0.418181818181818,0.422727272727273,0.427272727272727,0.431818181818182),
 .UNSPECIFIED.)
CURVE()
GEOMETRIC_REPRESENTATION_ITEM()
RATIONAL_B_SPLINE_CURVE((1.,0.951056516295154,1.,0.951056516295154,1.,0.951056516295154,
1.,0.951056516295154,1.,0.951056516295154,1.,0.951056516295154,1.,0.951056516295154,
1.,0.951056516295154,1.,0.951056516295154,1.,0.951056516295154,1.))
REPRESENTATION_ITEM('')
);
#475=(
BOUNDED_CURVE()
B_SPLINE_CURVE(2,(#23487,#23488,#23489,#23490,#23491,#23492,#23493,#23494,
#23495,#23496,#23497,#23498,#23499,#23500,#23501,#23502,#23503,#23504,#23505,
#23506,#23507),.UNSPECIFIED.,.F.,.F.)
B_SPLINE_CURVE_WITH_KNOTS((3,2,2,2,2,2,2,2,2,2,3),(0.392545981095113,0.397164169107997,
0.40178235712088,0.406400545133764,0.411018733146648,0.415636921159532,
0.420255109172415,0.424873297185299,0.429491485198183,0.434109673211066,
0.43872786122395),.UNSPECIFIED.)
CURVE()
GEOMETRIC_REPRESENTATION_ITEM()
RATIONAL_B_SPLINE_CURVE((1.,0.951056516295154,1.,0.951056516295154,1.,0.951056516295154,
1.,0.951056516295154,1.,0.951056516295154,1.,0.951056516295154,1.,0.951056516295154,
1.,0.951056516295154,1.,0.951056516295154,1.,0.951056516295154,1.))
REPRESENTATION_ITEM('')
);
#476=(
BOUNDED_CURVE()
B_SPLINE_CURVE(2,(#23512,#23513,#23514,#23515,#23516,#23517,#23518,#23519,
#23520,#23521,#23522,#23523,#23524,#23525,#23526,#23527,#23528,#23529,#23530,
#23531,#23532),.UNSPECIFIED.,.F.,.F.)
B_SPLINE_CURVE_WITH_KNOTS((3,2,2,2,2,2,2,2,2,2,3),(0.431818181818182,0.436363636363636,
0.440909090909091,0.445454545454545,0.45,0.454545454545455,0.459090909090909,
0.463636363636364,0.468181818181818,0.472727272727273,0.477272727272727),
 .UNSPECIFIED.)
CURVE()
GEOMETRIC_REPRESENTATION_ITEM()
RATIONAL_B_SPLINE_CURVE((1.,0.951056516295154,1.,0.951056516295154,1.,0.951056516295154,
1.,0.951056516295154,1.,0.951056516295154,1.,0.951056516295154,1.,0.951056516295154,
1.,0.951056516295154,1.,0.951056516295154,1.,0.951056516295154,1.))
REPRESENTATION_ITEM('')
);
#477=(
BOUNDED_CURVE()
B_SPLINE_CURVE(2,(#23533,#23534,#23535,#23536,#23537,#23538,#23539,#23540,
#23541,#23542,#23543,#23544,#23545,#23546,#23547,#23548,#23549,#23550,#23551,
#23552,#23553),.UNSPECIFIED.,.F.,.F.)
B_SPLINE_CURVE_WITH_KNOTS((3,2,2,2,2,2,2,2,2,2,3),(0.43872786122395,0.443346049236834,
0.447964237249717,0.452582425262601,0.457200613275485,0.461818801288368,
0.466436989301252,0.471055177314136,0.47567336532702,0.480291553339903,
0.484909741352787),.UNSPECIFIED.)
CURVE()
GEOMETRIC_REPRESENTATION_ITEM()
RATIONAL_B_SPLINE_CURVE((1.,0.951056516295154,1.,0.951056516295154,1.,0.951056516295154,
1.,0.951056516295154,1.,0.951056516295154,1.,0.951056516295154,1.,0.951056516295154,
1.,0.951056516295154,1.,0.951056516295154,1.,0.951056516295154,1.))
REPRESENTATION_ITEM('')
);
#478=(
BOUNDED_CURVE()
B_SPLINE_CURVE(2,(#23558,#23559,#23560,#23561,#23562,#23563,#23564,#23565,
#23566,#23567,#23568,#23569,#23570,#23571,#23572,#23573,#23574,#23575,#23576,
#23577,#23578),.UNSPECIFIED.,.F.,.F.)
B_SPLINE_CURVE_WITH_KNOTS((3,2,2,2,2,2,2,2,2,2,3),(0.477272727272727,0.481818181818182,
0.486363636363636,0.490909090909091,0.495454545454545,0.5,0.504545454545455,
0.509090909090909,0.513636363636364,0.518181818181818,0.522727272727273),
 .UNSPECIFIED.)
CURVE()
GEOMETRIC_REPRESENTATION_ITEM()
RATIONAL_B_SPLINE_CURVE((1.,0.951056516295154,1.,0.951056516295154,1.,0.951056516295154,
1.,0.951056516295154,1.,0.951056516295154,1.,0.951056516295154,1.,0.951056516295154,
1.,0.951056516295154,1.,0.951056516295154,1.,0.951056516295154,1.))
REPRESENTATION_ITEM('')
);
#479=(
BOUNDED_CURVE()
B_SPLINE_CURVE(2,(#23579,#23580,#23581,#23582,#23583,#23584,#23585,#23586,
#23587,#23588,#23589,#23590,#23591,#23592,#23593,#23594,#23595,#23596,#23597,
#23598,#23599),.UNSPECIFIED.,.F.,.F.)
B_SPLINE_CURVE_WITH_KNOTS((3,2,2,2,2,2,2,2,2,2,3),(0.484909741352787,0.489527929365671,
0.494146117378554,0.498764305391438,0.503382493404322,0.508000681417205,
0.512618869430089,0.517237057442973,0.521855245455856,0.52647343346874,
0.531091621481624),.UNSPECIFIED.)
CURVE()
GEOMETRIC_REPRESENTATION_ITEM()
RATIONAL_B_SPLINE_CURVE((1.,0.951056516295154,1.,0.951056516295154,1.,0.951056516295154,
1.,0.951056516295154,1.,0.951056516295154,1.,0.951056516295154,1.,0.951056516295154,
1.,0.951056516295154,1.,0.951056516295154,1.,0.951056516295154,1.))
REPRESENTATION_ITEM('')
);
#480=(
BOUNDED_CURVE()
B_SPLINE_CURVE(2,(#23604,#23605,#23606,#23607,#23608,#23609,#23610,#23611,
#23612,#23613,#23614,#23615,#23616,#23617,#23618,#23619,#23620,#23621,#23622,
#23623,#23624),.UNSPECIFIED.,.F.,.F.)
B_SPLINE_CURVE_WITH_KNOTS((3,2,2,2,2,2,2,2,2,2,3),(0.522727272727273,0.527272727272727,
0.531818181818182,0.536363636363636,0.540909090909091,0.545454545454545,
0.55,0.554545454545455,0.559090909090909,0.563636363636364,0.568181818181818),
 .UNSPECIFIED.)
CURVE()
GEOMETRIC_REPRESENTATION_ITEM()
RATIONAL_B_SPLINE_CURVE((1.,0.951056516295154,1.,0.951056516295154,1.,0.951056516295154,
1.,0.951056516295154,1.,0.951056516295154,1.,0.951056516295154,1.,0.951056516295154,
1.,0.951056516295154,1.,0.951056516295154,1.,0.951056516295154,1.))
REPRESENTATION_ITEM('')
);
#481=(
BOUNDED_CURVE()
B_SPLINE_CURVE(2,(#23625,#23626,#23627,#23628,#23629,#23630,#23631,#23632,
#23633,#23634,#23635,#23636,#23637,#23638,#23639,#23640,#23641,#23642,#23643,
#23644,#23645),.UNSPECIFIED.,.F.,.F.)
B_SPLINE_CURVE_WITH_KNOTS((3,2,2,2,2,2,2,2,2,2,3),(0.531091621481624,0.535709809494508,
0.540327997507391,0.544946185520275,0.549564373533159,0.554182561546042,
0.558800749558926,0.56341893757181,0.568037125584693,0.572655313597577,
0.577273501610461),.UNSPECIFIED.)
CURVE()
GEOMETRIC_REPRESENTATION_ITEM()
RATIONAL_B_SPLINE_CURVE((1.,0.951056516295154,1.,0.951056516295154,1.,0.951056516295154,
1.,0.951056516295154,1.,0.951056516295154,1.,0.951056516295154,1.,0.951056516295154,
1.,0.951056516295154,1.,0.951056516295154,1.,0.951056516295154,1.))
REPRESENTATION_ITEM('')
);
#482=(
BOUNDED_CURVE()
B_SPLINE_CURVE(2,(#23650,#23651,#23652,#23653,#23654,#23655,#23656,#23657,
#23658,#23659,#23660,#23661,#23662,#23663,#23664,#23665,#23666,#23667,#23668,
#23669,#23670),.UNSPECIFIED.,.F.,.F.)
B_SPLINE_CURVE_WITH_KNOTS((3,2,2,2,2,2,2,2,2,2,3),(0.568181818181818,0.572727272727273,
0.577272727272727,0.581818181818182,0.586363636363636,0.590909090909091,
0.595454545454546,0.6,0.604545454545454,0.609090909090909,0.613636363636364),
 .UNSPECIFIED.)
CURVE()
GEOMETRIC_REPRESENTATION_ITEM()
RATIONAL_B_SPLINE_CURVE((1.,0.951056516295154,1.,0.951056516295154,1.,0.951056516295154,
1.,0.951056516295154,1.,0.951056516295154,1.,0.951056516295154,1.,0.951056516295154,
1.,0.951056516295154,1.,0.951056516295154,1.,0.951056516295154,1.))
REPRESENTATION_ITEM('')
);
#483=(
BOUNDED_CURVE()
B_SPLINE_CURVE(2,(#23671,#23672,#23673,#23674,#23675,#23676,#23677,#23678,
#23679,#23680,#23681,#23682,#23683,#23684,#23685,#23686,#23687,#23688,#23689,
#23690,#23691),.UNSPECIFIED.,.F.,.F.)
B_SPLINE_CURVE_WITH_KNOTS((3,2,2,2,2,2,2,2,2,2,3),(0.577273501610461,0.581891689623344,
0.586509877636228,0.591128065649112,0.595746253661995,0.600364441674879,
0.604982629687763,0.609600817700647,0.61421900571353,0.618837193726414,
0.623455381739298),.UNSPECIFIED.)
CURVE()
GEOMETRIC_REPRESENTATION_ITEM()
RATIONAL_B_SPLINE_CURVE((1.,0.951056516295154,1.,0.951056516295154,1.,0.951056516295154,
1.,0.951056516295154,1.,0.951056516295154,1.,0.951056516295154,1.,0.951056516295154,
1.,0.951056516295154,1.,0.951056516295154,1.,0.951056516295154,1.))
REPRESENTATION_ITEM('')
);
#484=(
BOUNDED_CURVE()
B_SPLINE_CURVE(2,(#23696,#23697,#23698,#23699,#23700,#23701,#23702,#23703,
#23704,#23705,#23706,#23707,#23708,#23709,#23710,#23711,#23712,#23713,#23714,
#23715,#23716),.UNSPECIFIED.,.F.,.F.)
B_SPLINE_CURVE_WITH_KNOTS((3,2,2,2,2,2,2,2,2,2,3),(0.613636363636364,0.618181818181818,
0.622727272727273,0.627272727272727,0.631818181818182,0.636363636363636,
0.640909090909091,0.645454545454546,0.65,0.654545454545455,0.659090909090909),
 .UNSPECIFIED.)
CURVE()
GEOMETRIC_REPRESENTATION_ITEM()
RATIONAL_B_SPLINE_CURVE((1.,0.951056516295154,1.,0.951056516295154,1.,0.951056516295154,
1.,0.951056516295154,1.,0.951056516295154,1.,0.951056516295154,1.,0.951056516295154,
1.,0.951056516295154,1.,0.951056516295154,1.,0.951056516295154,1.))
REPRESENTATION_ITEM('')
);
#485=(
BOUNDED_CURVE()
B_SPLINE_CURVE(2,(#23717,#23718,#23719,#23720,#23721,#23722,#23723,#23724,
#23725,#23726,#23727,#23728,#23729,#23730,#23731,#23732,#23733,#23734,#23735,
#23736,#23737),.UNSPECIFIED.,.F.,.F.)
B_SPLINE_CURVE_WITH_KNOTS((3,2,2,2,2,2,2,2,2,2,3),(0.623455381739298,0.628073569752181,
0.632691757765065,0.637309945777949,0.641928133790832,0.646546321803716,
0.6511645098166,0.655782697829484,0.660400885842367,0.665019073855251,0.669637261868135),
 .UNSPECIFIED.)
CURVE()
GEOMETRIC_REPRESENTATION_ITEM()
RATIONAL_B_SPLINE_CURVE((1.,0.951056516295154,1.,0.951056516295154,1.,0.951056516295154,
1.,0.951056516295154,1.,0.951056516295154,1.,0.951056516295154,1.,0.951056516295154,
1.,0.951056516295154,1.,0.951056516295154,1.,0.951056516295154,1.))
REPRESENTATION_ITEM('')
);
#486=(
BOUNDED_CURVE()
B_SPLINE_CURVE(2,(#23742,#23743,#23744,#23745,#23746,#23747,#23748,#23749,
#23750,#23751,#23752,#23753,#23754,#23755,#23756,#23757,#23758,#23759,#23760,
#23761,#23762),.UNSPECIFIED.,.F.,.F.)
B_SPLINE_CURVE_WITH_KNOTS((3,2,2,2,2,2,2,2,2,2,3),(0.659090909090909,0.663636363636364,
0.668181818181818,0.672727272727273,0.677272727272727,0.681818181818182,
0.686363636363636,0.690909090909091,0.695454545454545,0.7,0.704545454545455),
 .UNSPECIFIED.)
CURVE()
GEOMETRIC_REPRESENTATION_ITEM()
RATIONAL_B_SPLINE_CURVE((1.,0.951056516295154,1.,0.951056516295154,1.,0.951056516295154,
1.,0.951056516295154,1.,0.951056516295154,1.,0.951056516295154,1.,0.951056516295154,
1.,0.951056516295154,1.,0.951056516295154,1.,0.951056516295154,1.))
REPRESENTATION_ITEM('')
);
#487=(
BOUNDED_CURVE()
B_SPLINE_CURVE(2,(#23763,#23764,#23765,#23766,#23767,#23768,#23769,#23770,
#23771,#23772,#23773,#23774,#23775,#23776,#23777,#23778,#23779,#23780,#23781,
#23782,#23783),.UNSPECIFIED.,.F.,.F.)
B_SPLINE_CURVE_WITH_KNOTS((3,2,2,2,2,2,2,2,2,2,3),(0.669637261868135,0.674255449881018,
0.678873637893902,0.683491825906786,0.688110013919669,0.692728201932553,
0.697346389945437,0.70196457795832,0.706582765971204,0.711200953984088,
0.715819141996971),.UNSPECIFIED.)
CURVE()
GEOMETRIC_REPRESENTATION_ITEM()
RATIONAL_B_SPLINE_CURVE((1.,0.951056516295154,1.,0.951056516295154,1.,0.951056516295154,
1.,0.951056516295154,1.,0.951056516295154,1.,0.951056516295154,1.,0.951056516295154,
1.,0.951056516295154,1.,0.951056516295154,1.,0.951056516295154,1.))
REPRESENTATION_ITEM('')
);
#488=(
BOUNDED_CURVE()
B_SPLINE_CURVE(2,(#23788,#23789,#23790,#23791,#23792,#23793,#23794,#23795,
#23796,#23797,#23798,#23799,#23800,#23801,#23802,#23803,#23804,#23805,#23806,
#23807,#23808),.UNSPECIFIED.,.F.,.F.)
B_SPLINE_CURVE_WITH_KNOTS((3,2,2,2,2,2,2,2,2,2,3),(0.704545454545455,0.709090909090909,
0.713636363636364,0.718181818181818,0.722727272727273,0.727272727272727,
0.731818181818182,0.736363636363636,0.740909090909091,0.745454545454545,
0.75),.UNSPECIFIED.)
CURVE()
GEOMETRIC_REPRESENTATION_ITEM()
RATIONAL_B_SPLINE_CURVE((1.,0.951056516295154,1.,0.951056516295154,1.,0.951056516295154,
1.,0.951056516295154,1.,0.951056516295154,1.,0.951056516295154,1.,0.951056516295154,
1.,0.951056516295154,1.,0.951056516295154,1.,0.951056516295154,1.))
REPRESENTATION_ITEM('')
);
#489=(
BOUNDED_CURVE()
B_SPLINE_CURVE(2,(#23809,#23810,#23811,#23812,#23813,#23814,#23815,#23816,
#23817,#23818,#23819,#23820,#23821,#23822,#23823,#23824,#23825,#23826,#23827,
#23828,#23829),.UNSPECIFIED.,.F.,.F.)
B_SPLINE_CURVE_WITH_KNOTS((3,2,2,2,2,2,2,2,2,2,3),(0.715819141996971,0.720437330009855,
0.725055518022739,0.729673706035622,0.734291894048506,0.73891008206139,
0.743528270074274,0.748146458087157,0.752764646100041,0.757382834112925,
0.762001022125808),.UNSPECIFIED.)
CURVE()
GEOMETRIC_REPRESENTATION_ITEM()
RATIONAL_B_SPLINE_CURVE((1.,0.951056516295154,1.,0.951056516295154,1.,0.951056516295154,
1.,0.951056516295154,1.,0.951056516295154,1.,0.951056516295154,1.,0.951056516295154,
1.,0.951056516295154,1.,0.951056516295154,1.,0.951056516295154,1.))
REPRESENTATION_ITEM('')
);
#490=(
BOUNDED_CURVE()
B_SPLINE_CURVE(2,(#23834,#23835,#23836,#23837,#23838,#23839,#23840,#23841,
#23842,#23843,#23844,#23845,#23846,#23847,#23848,#23849,#23850,#23851,#23852,
#23853,#23854),.UNSPECIFIED.,.F.,.F.)
B_SPLINE_CURVE_WITH_KNOTS((3,2,2,2,2,2,2,2,2,2,3),(0.75,0.754545454545455,
0.759090909090909,0.763636363636364,0.768181818181818,0.772727272727273,
0.777272727272727,0.781818181818182,0.786363636363636,0.790909090909091,
0.795454545454545),.UNSPECIFIED.)
CURVE()
GEOMETRIC_REPRESENTATION_ITEM()
RATIONAL_B_SPLINE_CURVE((1.,0.951056516295154,1.,0.951056516295154,1.,0.951056516295154,
1.,0.951056516295154,1.,0.951056516295154,1.,0.951056516295154,1.,0.951056516295154,
1.,0.951056516295154,1.,0.951056516295154,1.,0.951056516295154,1.))
REPRESENTATION_ITEM('')
);
#491=(
BOUNDED_CURVE()
B_SPLINE_CURVE(2,(#23855,#23856,#23857,#23858,#23859,#23860,#23861,#23862,
#23863,#23864,#23865,#23866,#23867,#23868,#23869,#23870,#23871,#23872,#23873,
#23874,#23875),.UNSPECIFIED.,.F.,.F.)
B_SPLINE_CURVE_WITH_KNOTS((3,2,2,2,2,2,2,2,2,2,3),(0.762001022125808,0.766619210138692,
0.771237398151576,0.775855586164459,0.780473774177343,0.785091962190227,
0.78971015020311,0.794328338215994,0.798946526228878,0.803564714241761,
0.808182902254645),.UNSPECIFIED.)
CURVE()
GEOMETRIC_REPRESENTATION_ITEM()
RATIONAL_B_SPLINE_CURVE((1.,0.951056516295154,1.,0.951056516295154,1.,0.951056516295154,
1.,0.951056516295154,1.,0.951056516295154,1.,0.951056516295154,1.,0.951056516295154,
1.,0.951056516295154,1.,0.951056516295154,1.,0.951056516295154,1.))
REPRESENTATION_ITEM('')
);
#492=(
BOUNDED_CURVE()
B_SPLINE_CURVE(2,(#23880,#23881,#23882,#23883,#23884,#23885,#23886,#23887,
#23888,#23889,#23890,#23891,#23892,#23893,#23894,#23895,#23896,#23897,#23898,
#23899,#23900),.UNSPECIFIED.,.F.,.F.)
B_SPLINE_CURVE_WITH_KNOTS((3,2,2,2,2,2,2,2,2,2,3),(0.795454545454545,0.8,
0.804545454545455,0.809090909090909,0.813636363636364,0.818181818181818,
0.822727272727273,0.827272727272727,0.831818181818182,0.836363636363636,
0.840909090909091),.UNSPECIFIED.)
CURVE()
GEOMETRIC_REPRESENTATION_ITEM()
RATIONAL_B_SPLINE_CURVE((1.,0.951056516295154,1.,0.951056516295154,1.,0.951056516295154,
1.,0.951056516295154,1.,0.951056516295154,1.,0.951056516295154,1.,0.951056516295154,
1.,0.951056516295154,1.,0.951056516295154,1.,0.951056516295154,1.))
REPRESENTATION_ITEM('')
);
#493=(
BOUNDED_CURVE()
B_SPLINE_CURVE(2,(#23901,#23902,#23903,#23904,#23905,#23906,#23907,#23908,
#23909,#23910,#23911,#23912,#23913,#23914,#23915,#23916,#23917,#23918,#23919,
#23920,#23921),.UNSPECIFIED.,.F.,.F.)
B_SPLINE_CURVE_WITH_KNOTS((3,2,2,2,2,2,2,2,2,2,3),(0.808182902254645,0.812801090267529,
0.817419278280413,0.822037466293296,0.82665565430618,0.831273842319064,
0.835892030331947,0.840510218344831,0.845128406357715,0.849746594370598,
0.854364782383482),.UNSPECIFIED.)
CURVE()
GEOMETRIC_REPRESENTATION_ITEM()
RATIONAL_B_SPLINE_CURVE((1.,0.951056516295154,1.,0.951056516295154,1.,0.951056516295154,
1.,0.951056516295154,1.,0.951056516295154,1.,0.951056516295154,1.,0.951056516295154,
1.,0.951056516295154,1.,0.951056516295154,1.,0.951056516295154,1.))
REPRESENTATION_ITEM('')
);
#494=(
BOUNDED_CURVE()
B_SPLINE_CURVE(2,(#23926,#23927,#23928,#23929,#23930,#23931,#23932,#23933,
#23934,#23935,#23936,#23937,#23938,#23939,#23940,#23941,#23942,#23943,#23944,
#23945,#23946),.UNSPECIFIED.,.F.,.F.)
B_SPLINE_CURVE_WITH_KNOTS((3,2,2,2,2,2,2,2,2,2,3),(0.840909090909091,0.845454545454545,
0.85,0.854545454545454,0.859090909090909,0.863636363636364,0.868181818181818,
0.872727272727273,0.877272727272727,0.881818181818182,0.886363636363636),
 .UNSPECIFIED.)
CURVE()
GEOMETRIC_REPRESENTATION_ITEM()
RATIONAL_B_SPLINE_CURVE((1.,0.951056516295154,1.,0.951056516295154,1.,0.951056516295154,
1.,0.951056516295154,1.,0.951056516295154,1.,0.951056516295154,1.,0.951056516295154,
1.,0.951056516295154,1.,0.951056516295154,1.,0.951056516295154,1.))
REPRESENTATION_ITEM('')
);
#495=(
BOUNDED_CURVE()
B_SPLINE_CURVE(2,(#23947,#23948,#23949,#23950,#23951,#23952,#23953,#23954,
#23955,#23956,#23957,#23958,#23959,#23960,#23961,#23962,#23963,#23964,#23965,
#23966,#23967),.UNSPECIFIED.,.F.,.F.)
B_SPLINE_CURVE_WITH_KNOTS((3,2,2,2,2,2,2,2,2,2,3),(0.854364782383482,0.858982970396366,
0.863601158409249,0.868219346422133,0.872837534435017,0.877455722447901,
0.882073910460784,0.886692098473668,0.891310286486552,0.895928474499435,
0.900546662512319),.UNSPECIFIED.)
CURVE()
GEOMETRIC_REPRESENTATION_ITEM()
RATIONAL_B_SPLINE_CURVE((1.,0.951056516295154,1.,0.951056516295154,1.,0.951056516295154,
1.,0.951056516295154,1.,0.951056516295154,1.,0.951056516295154,1.,0.951056516295154,
1.,0.951056516295154,1.,0.951056516295154,1.,0.951056516295154,1.))
REPRESENTATION_ITEM('')
);
#496=(
BOUNDED_CURVE()
B_SPLINE_CURVE(2,(#23972,#23973,#23974,#23975,#23976,#23977,#23978,#23979,
#23980,#23981,#23982,#23983,#23984,#23985,#23986,#23987,#23988,#23989,#23990,
#23991,#23992),.UNSPECIFIED.,.F.,.F.)
B_SPLINE_CURVE_WITH_KNOTS((3,2,2,2,2,2,2,2,2,2,3),(0.886363636363636,0.890909090909091,
0.895454545454546,0.9,0.904545454545455,0.909090909090909,0.913636363636364,
0.918181818181818,0.922727272727273,0.927272727272727,0.931818181818182),
 .UNSPECIFIED.)
CURVE()
GEOMETRIC_REPRESENTATION_ITEM()
RATIONAL_B_SPLINE_CURVE((1.,0.951056516295154,1.,0.951056516295154,1.,0.951056516295154,
1.,0.951056516295154,1.,0.951056516295154,1.,0.951056516295154,1.,0.951056516295154,
1.,0.951056516295154,1.,0.951056516295154,1.,0.951056516295154,1.))
REPRESENTATION_ITEM('')
);
#497=(
BOUNDED_CURVE()
B_SPLINE_CURVE(2,(#23993,#23994,#23995,#23996,#23997,#23998,#23999,#24000,
#24001,#24002,#24003,#24004,#24005,#24006,#24007,#24008,#24009,#24010,#24011,
#24012,#24013),.UNSPECIFIED.,.F.,.F.)
B_SPLINE_CURVE_WITH_KNOTS((3,2,2,2,2,2,2,2,2,2,3),(0.900546662512319,0.905164850525203,
0.909783038538087,0.91440122655097,0.919019414563854,0.923637602576737,
0.928255790589621,0.932873978602505,0.937492166615388,0.942110354628272,
0.946728542641156),.UNSPECIFIED.)
CURVE()
GEOMETRIC_REPRESENTATION_ITEM()
RATIONAL_B_SPLINE_CURVE((1.,0.951056516295154,1.,0.951056516295154,1.,0.951056516295154,
1.,0.951056516295154,1.,0.951056516295154,1.,0.951056516295154,1.,0.951056516295154,
1.,0.951056516295154,1.,0.951056516295154,1.,0.951056516295154,1.))
REPRESENTATION_ITEM('')
);
#498=(
BOUNDED_CURVE()
B_SPLINE_CURVE(2,(#24018,#24019,#24020,#24021,#24022,#24023,#24024,#24025,
#24026,#24027,#24028,#24029,#24030,#24031,#24032,#24033,#24034,#24035,#24036,
#24037,#24038),.UNSPECIFIED.,.F.,.F.)
B_SPLINE_CURVE_WITH_KNOTS((3,2,2,2,2,2,2,2,2,2,3),(0.931818181818182,0.936363636363636,
0.940909090909091,0.945454545454545,0.95,0.954545454545455,0.959090909090909,
0.963636363636364,0.968181818181818,0.972727272727273,0.977272727272727),
 .UNSPECIFIED.)
CURVE()
GEOMETRIC_REPRESENTATION_ITEM()
RATIONAL_B_SPLINE_CURVE((1.,0.951056516295154,1.,0.951056516295154,1.,0.951056516295154,
1.,0.951056516295154,1.,0.951056516295154,1.,0.951056516295154,1.,0.951056516295154,
1.,0.951056516295154,1.,0.951056516295154,1.,0.951056516295154,1.))
REPRESENTATION_ITEM('')
);
#499=(
BOUNDED_CURVE()
B_SPLINE_CURVE(2,(#24039,#24040,#24041,#24042,#24043,#24044,#24045,#24046,
#24047,#24048,#24049,#24050,#24051,#24052,#24053,#24054,#24055,#24056,#24057,
#24058,#24059),.UNSPECIFIED.,.F.,.F.)
B_SPLINE_CURVE_WITH_KNOTS((3,2,2,2,2,2,2,2,2,2,3),(0.946728542641156,0.95134673065404,
0.955964918666923,0.960583106679807,0.965201294692691,0.969819482705574,
0.974437670718458,0.979055858731342,0.983674046744225,0.988292234757109,
0.992910422769993),.UNSPECIFIED.)
CURVE()
GEOMETRIC_REPRESENTATION_ITEM()
RATIONAL_B_SPLINE_CURVE((1.,0.951056516295154,1.,0.951056516295154,1.,0.951056516295154,
1.,0.951056516295154,1.,0.951056516295154,1.,0.951056516295154,1.,0.951056516295154,
1.,0.951056516295154,1.,0.951056516295154,1.,0.951056516295154,1.))
REPRESENTATION_ITEM('')
);
#500=(
BOUNDED_CURVE()
B_SPLINE_CURVE(2,(#27442,#27443,#27444,#27445,#27446),.UNSPECIFIED.,.F.,
 .F.)
B_SPLINE_CURVE_WITH_KNOTS((3,2,3),(0.992910422769993,0.997528610782876,
0.999999992267812),.UNSPECIFIED.)
CURVE()
GEOMETRIC_REPRESENTATION_ITEM()
RATIONAL_B_SPLINE_CURVE((1.,0.951056516295154,1.,0.973808338010719,0.975649137376158))
REPRESENTATION_ITEM('')
);
#501=(
BOUNDED_CURVE()
B_SPLINE_CURVE(2,(#27448,#27449,#27450,#27451,#27452),.UNSPECIFIED.,.F.,
 .F.)
B_SPLINE_CURVE_WITH_KNOTS((3,2,3),(0.977272727272727,0.981818181818182,
0.984250640944397),.UNSPECIFIED.)
CURVE()
GEOMETRIC_REPRESENTATION_ITEM()
RATIONAL_B_SPLINE_CURVE((1.,0.951056516295154,1.,0.973808334806544,0.975649137826549))
REPRESENTATION_ITEM('')
);
#502=(
BOUNDED_CURVE()
B_SPLINE_CURVE(2,(#29145,#29146,#29147,#29148,#29149,#29150,#29151,#29152,
#29153,#29154,#29155,#29156,#29157,#29158,#29159),.UNSPECIFIED.,.F.,.F.)
B_SPLINE_CURVE_WITH_KNOTS((3,2,2,2,2,2,2,3),(0.816943476460579,0.831796994214408,
0.846650511968236,0.861504029722065,0.876357547475894,0.891211065229723,
0.906064582983552,0.916368765855157),.UNSPECIFIED.)
CURVE()
GEOMETRIC_REPRESENTATION_ITEM()
RATIONAL_B_SPLINE_CURVE((1.,0.951056516295154,1.,0.951056516295154,1.,0.951056516295154,
1.,0.951056516295154,1.,0.951056516295154,1.,0.951056516295154,1.,0.966046924720029,
0.979201706654285))
REPRESENTATION_ITEM('')
);
#503=(
BOUNDED_CURVE()
B_SPLINE_CURVE(2,(#29162,#29163,#29164,#29165,#29166,#29167,#29168,#29169,
#29170,#29171,#29172,#29173,#29174,#29175,#29176,#29177,#29178,#29179,#29180,
#29181,#29182),.UNSPECIFIED.,.F.,.F.)
B_SPLINE_CURVE_WITH_KNOTS((3,2,2,2,2,2,2,2,2,2,3),(0.785714285714286,0.8,
0.814285714285714,0.828571428571429,0.842857142857143,0.857142857142857,
0.871428571428571,0.885714285714286,0.9,0.914285714285714,0.917180190333488),
 .UNSPECIFIED.)
CURVE()
GEOMETRIC_REPRESENTATION_ITEM()
RATIONAL_B_SPLINE_CURVE((1.,0.951056516295154,1.,0.951056516295154,1.,0.951056516295154,
1.,0.951056516295154,1.,0.951056516295154,1.,0.951056516295154,1.,0.951056516295154,
1.,0.951056516295154,1.,0.951056516295154,1.,0.99008339811052,0.984185267551257))
REPRESENTATION_ITEM('')
);
#504=(
BOUNDED_CURVE()
B_SPLINE_CURVE(2,(#29187,#29188,#29189,#29190,#29191,#29192,#29193,#29194,
#29195,#29196,#29197,#29198,#29199,#29200,#29201,#29202,#29203,#29204,#29205,
#29206,#29207),.UNSPECIFIED.,.F.,.F.)
B_SPLINE_CURVE_WITH_KNOTS((3,2,2,2,2,2,2,2,2,2,3),(0.66840829892229,0.683261816676119,
0.698115334429948,0.712968852183777,0.727822369937606,0.742675887691435,
0.757529405445263,0.772382923199092,0.787236440952921,0.80208995870675,
0.816943476460579),.UNSPECIFIED.)
CURVE()
GEOMETRIC_REPRESENTATION_ITEM()
RATIONAL_B_SPLINE_CURVE((1.,0.951056516295154,1.,0.951056516295154,1.,0.951056516295154,
1.,0.951056516295154,1.,0.951056516295154,1.,0.951056516295154,1.,0.951056516295154,
1.,0.951056516295154,1.,0.951056516295154,1.,0.951056516295154,1.))
REPRESENTATION_ITEM('')
);
#505=(
BOUNDED_CURVE()
B_SPLINE_CURVE(2,(#29208,#29209,#29210,#29211,#29212,#29213,#29214,#29215,
#29216,#29217,#29218,#29219,#29220,#29221,#29222,#29223,#29224,#29225,#29226,
#29227,#29228),.UNSPECIFIED.,.F.,.F.)
B_SPLINE_CURVE_WITH_KNOTS((3,2,2,2,2,2,2,2,2,2,3),(0.642857142857143,0.657142857142857,
0.671428571428571,0.685714285714286,0.7,0.714285714285714,0.728571428571429,
0.742857142857143,0.757142857142857,0.771428571428571,0.785714285714286),
 .UNSPECIFIED.)
CURVE()
GEOMETRIC_REPRESENTATION_ITEM()
RATIONAL_B_SPLINE_CURVE((1.,0.951056516295154,1.,0.951056516295154,1.,0.951056516295154,
1.,0.951056516295154,1.,0.951056516295154,1.,0.951056516295154,1.,0.951056516295154,
1.,0.951056516295154,1.,0.951056516295154,1.,0.951056516295154,1.))
REPRESENTATION_ITEM('')
);
#506=(
BOUNDED_CURVE()
B_SPLINE_CURVE(2,(#29233,#29234,#29235,#29236,#29237,#29238,#29239,#29240,
#29241,#29242,#29243,#29244,#29245,#29246,#29247,#29248,#29249,#29250,#29251,
#29252,#29253),.UNSPECIFIED.,.F.,.F.)
B_SPLINE_CURVE_WITH_KNOTS((3,2,2,2,2,2,2,2,2,2,3),(0.519873121384002,0.534726639137831,
0.54958015689166,0.564433674645489,0.579287192399317,0.594140710153146,
0.608994227906975,0.623847745660804,0.638701263414633,0.653554781168462,
0.66840829892229),.UNSPECIFIED.)
CURVE()
GEOMETRIC_REPRESENTATION_ITEM()
RATIONAL_B_SPLINE_CURVE((1.,0.951056516295154,1.,0.951056516295154,1.,0.951056516295154,
1.,0.951056516295154,1.,0.951056516295154,1.,0.951056516295154,1.,0.951056516295154,
1.,0.951056516295154,1.,0.951056516295154,1.,0.951056516295154,1.))
REPRESENTATION_ITEM('')
);
#507=(
BOUNDED_CURVE()
B_SPLINE_CURVE(2,(#29254,#29255,#29256,#29257,#29258,#29259,#29260,#29261,
#29262,#29263,#29264,#29265,#29266,#29267,#29268,#29269,#29270,#29271,#29272,
#29273,#29274),.UNSPECIFIED.,.F.,.F.)
B_SPLINE_CURVE_WITH_KNOTS((3,2,2,2,2,2,2,2,2,2,3),(0.5,0.514285714285714,
0.528571428571429,0.542857142857143,0.557142857142857,0.571428571428571,
0.585714285714286,0.6,0.614285714285714,0.628571428571429,0.642857142857143),
 .UNSPECIFIED.)
CURVE()
GEOMETRIC_REPRESENTATION_ITEM()
RATIONAL_B_SPLINE_CURVE((1.,0.951056516295154,1.,0.951056516295154,1.,0.951056516295154,
1.,0.951056516295154,1.,0.951056516295154,1.,0.951056516295154,1.,0.951056516295154,
1.,0.951056516295154,1.,0.951056516295154,1.,0.951056516295154,1.))
REPRESENTATION_ITEM('')
);
#508=(
BOUNDED_CURVE()
B_SPLINE_CURVE(2,(#29279,#29280,#29281,#29282,#29283,#29284,#29285,#29286,
#29287,#29288,#29289,#29290,#29291,#29292,#29293,#29294,#29295,#29296,#29297,
#29298,#29299),.UNSPECIFIED.,.F.,.F.)
B_SPLINE_CURVE_WITH_KNOTS((3,2,2,2,2,2,2,2,2,2,3),(0.371337943845714,0.386191461599543,
0.401044979353371,0.4158984971072,0.430752014861029,0.445605532614858,0.460459050368687,
0.475312568122516,0.490166085876344,0.505019603630173,0.519873121384002),
 .UNSPECIFIED.)
CURVE()
GEOMETRIC_REPRESENTATION_ITEM()
RATIONAL_B_SPLINE_CURVE((1.,0.951056516295154,1.,0.951056516295154,1.,0.951056516295154,
1.,0.951056516295154,1.,0.951056516295154,1.,0.951056516295154,1.,0.951056516295154,
1.,0.951056516295154,1.,0.951056516295154,1.,0.951056516295154,1.))
REPRESENTATION_ITEM('')
);
#509=(
BOUNDED_CURVE()
B_SPLINE_CURVE(2,(#29300,#29301,#29302,#29303,#29304,#29305,#29306,#29307,
#29308,#29309,#29310,#29311,#29312,#29313,#29314,#29315,#29316,#29317,#29318,
#29319,#29320),.UNSPECIFIED.,.F.,.F.)
B_SPLINE_CURVE_WITH_KNOTS((3,2,2,2,2,2,2,2,2,2,3),(0.357142857142857,0.371428571428571,
0.385714285714286,0.4,0.414285714285714,0.428571428571428,0.442857142857143,
0.457142857142857,0.471428571428571,0.485714285714286,0.5),
 .UNSPECIFIED.)
CURVE()
GEOMETRIC_REPRESENTATION_ITEM()
RATIONAL_B_SPLINE_CURVE((1.,0.951056516295154,1.,0.951056516295154,1.,0.951056516295154,
1.,0.951056516295154,1.,0.951056516295154,1.,0.951056516295154,1.,0.951056516295154,
1.,0.951056516295154,1.,0.951056516295154,1.,0.951056516295154,1.))
REPRESENTATION_ITEM('')
);
#510=(
BOUNDED_CURVE()
B_SPLINE_CURVE(2,(#29326,#29327,#29328,#29329,#29330,#29331,#29332,#29333,
#29334,#29335,#29336,#29337,#29338,#29339,#29340),.UNSPECIFIED.,.F.,.F.)
B_SPLINE_CURVE_WITH_KNOTS((3,2,2,2,2,2,2,3),(0.124029642498174,0.128571428571429,
0.142857142857143,0.157142857142857,0.171428571428571,0.185714285714286,
0.2,0.214285714285714),.UNSPECIFIED.)
CURVE()
GEOMETRIC_REPRESENTATION_ITEM()
RATIONAL_B_SPLINE_CURVE((0.978773338025185,0.984439641713294,1.,0.951056516295154,
1.,0.951056516295154,1.,0.951056516295154,1.,0.951056516295154,1.,0.951056516295154,
1.,0.951056516295154,1.))
REPRESENTATION_ITEM('')
);
#511=(
BOUNDED_CURVE()
B_SPLINE_CURVE(2,(#29343,#29344,#29345,#29346,#29347,#29348,#29349,#29350,
#29351,#29352,#29353,#29354,#29355,#29356,#29357,#29358,#29359,#29360,#29361),
 .UNSPECIFIED.,.F.,.F.)
B_SPLINE_CURVE_WITH_KNOTS((3,2,2,2,2,2,2,2,2,3),(0.091954686099144,0.103974624276795,
0.118828142030624,0.133681659784452,0.148535177538281,0.16338869529211,
0.178242213045939,0.193095730799768,0.207949248553597,0.222802766307425),
 .UNSPECIFIED.)
CURVE()
GEOMETRIC_REPRESENTATION_ITEM()
RATIONAL_B_SPLINE_CURVE((0.984888628507613,0.96039337899068,1.,0.951056516295154,
1.,0.951056516295154,1.,0.951056516295154,1.,0.951056516295154,1.,0.951056516295154,
1.,0.951056516295154,1.,0.951056516295154,1.,0.951056516295154,1.))
REPRESENTATION_ITEM('')
);
#512=(
BOUNDED_CURVE()
B_SPLINE_CURVE(2,(#29757,#29758,#29759),.UNSPECIFIED.,.F.,.F.)
B_SPLINE_CURVE_WITH_KNOTS((3,3),(1.62371575593398,2.33717063536819),
 .UNSPECIFIED.)
CURVE()
GEOMETRIC_REPRESENTATION_ITEM()
RATIONAL_B_SPLINE_CURVE((1.32286062935255,1.34451361022803,1.32286062935255))
REPRESENTATION_ITEM('')
);
#513=(
BOUNDED_CURVE()
B_SPLINE_CURVE(2,(#29846,#29847,#29848),.UNSPECIFIED.,.F.,.F.)
B_SPLINE_CURVE_WITH_KNOTS((3,3),(2.20401193750953,2.35502343804526),
 .UNSPECIFIED.)
CURVE()
GEOMETRIC_REPRESENTATION_ITEM()
RATIONAL_B_SPLINE_CURVE((1.61068751795193,1.61882963884505,1.62522061017657))
REPRESENTATION_ITEM('')
);
#514=(
BOUNDED_CURVE()
B_SPLINE_CURVE(2,(#29856,#29857,#29858),.UNSPECIFIED.,.F.,.F.)
B_SPLINE_CURVE_WITH_KNOTS((3,3),(-2.35502343804526,-1.66463996329892),
 .UNSPECIFIED.)
CURVE()
GEOMETRIC_REPRESENTATION_ITEM()
RATIONAL_B_SPLINE_CURVE((1.62522061017657,1.59600282888702,1.53018480461537))
REPRESENTATION_ITEM('')
);
#515=(
BOUNDED_CURVE()
B_SPLINE_CURVE(2,(#29862,#29863,#29864),.UNSPECIFIED.,.F.,.F.)
B_SPLINE_CURVE_WITH_KNOTS((3,3),(-4.14763863034457,-3.45725829975021),
 .UNSPECIFIED.)
CURVE()
GEOMETRIC_REPRESENTATION_ITEM()
RATIONAL_B_SPLINE_CURVE((1.53017908155183,1.59599685965665,1.62521453166841))
REPRESENTATION_ITEM('')
);
#516=(
BOUNDED_CURVE()
B_SPLINE_CURVE(2,(#29868,#29869,#29870),.UNSPECIFIED.,.F.,.F.)
B_SPLINE_CURVE_WITH_KNOTS((3,3),(-2.35500433297853,-1.66462400238418),
 .UNSPECIFIED.)
CURVE()
GEOMETRIC_REPRESENTATION_ITEM()
RATIONAL_B_SPLINE_CURVE((1.62521453166841,1.59599685965665,1.53017908155183))
REPRESENTATION_ITEM('')
);
#517=(
BOUNDED_CURVE()
B_SPLINE_CURVE(2,(#29880,#29881,#29882),.UNSPECIFIED.,.F.,.F.)
B_SPLINE_CURVE_WITH_KNOTS((3,3),(-4.1476561584474,-3.45727380684988),
 .UNSPECIFIED.)
CURVE()
GEOMETRIC_REPRESENTATION_ITEM()
RATIONAL_B_SPLINE_CURVE((1.53018276023192,1.59600069656826,1.62521843882178))
REPRESENTATION_ITEM('')
);
#518=(
BOUNDED_CURVE()
B_SPLINE_CURVE(2,(#29886,#29887,#29888),.UNSPECIFIED.,.F.,.F.)
B_SPLINE_CURVE_WITH_KNOTS((3,3),(-2.35501661336581,-1.66463426176827),
 .UNSPECIFIED.)
CURVE()
GEOMETRIC_REPRESENTATION_ITEM()
RATIONAL_B_SPLINE_CURVE((1.62521843882178,1.59600069656826,1.53018276023192))
REPRESENTATION_ITEM('')
);
#519=(
BOUNDED_CURVE()
B_SPLINE_CURVE(2,(#29892,#29893,#29894),.UNSPECIFIED.,.F.,.F.)
B_SPLINE_CURVE_WITH_KNOTS((3,3),(-4.14763863034456,-3.45725829975022),
 .UNSPECIFIED.)
CURVE()
GEOMETRIC_REPRESENTATION_ITEM()
RATIONAL_B_SPLINE_CURVE((1.53017908155184,1.59599685965666,1.62521453166842))
REPRESENTATION_ITEM('')
);
#520=(
BOUNDED_CURVE()
B_SPLINE_CURVE(2,(#30008,#30009,#30010),.UNSPECIFIED.,.F.,.F.)
B_SPLINE_CURVE_WITH_KNOTS((3,3),(-4.14765638055873,-3.45727400335158),
 .UNSPECIFIED.)
CURVE()
GEOMETRIC_REPRESENTATION_ITEM()
RATIONAL_B_SPLINE_CURVE((1.53018280684717,1.59600074518857,1.62521848833218))
REPRESENTATION_ITEM('')
);
#521=(
BOUNDED_CURVE()
B_SPLINE_CURVE(2,(#30011,#30012,#30013),.UNSPECIFIED.,.F.,.F.)
B_SPLINE_CURVE_WITH_KNOTS((3,3),(-2.35501676897952,-1.66463439177237),
 .UNSPECIFIED.)
CURVE()
GEOMETRIC_REPRESENTATION_ITEM()
RATIONAL_B_SPLINE_CURVE((1.62521848833218,1.59600074518857,1.53018280684717))
REPRESENTATION_ITEM('')
);
#522=(
BOUNDED_CURVE()
B_SPLINE_CURVE(2,(#30014,#30015,#30016),.UNSPECIFIED.,.F.,.F.)
B_SPLINE_CURVE_WITH_KNOTS((3,3),(-4.14763863034456,-3.45725829975021),
 .UNSPECIFIED.)
CURVE()
GEOMETRIC_REPRESENTATION_ITEM()
RATIONAL_B_SPLINE_CURVE((1.53017908155183,1.59599685965666,1.62521453166841))
REPRESENTATION_ITEM('')
);
#523=(
BOUNDED_CURVE()
B_SPLINE_CURVE(2,(#30017,#30018,#30019),.UNSPECIFIED.,.F.,.F.)
B_SPLINE_CURVE_WITH_KNOTS((3,3),(-2.35500433297852,-1.66462400238418),
 .UNSPECIFIED.)
CURVE()
GEOMETRIC_REPRESENTATION_ITEM()
RATIONAL_B_SPLINE_CURVE((1.62521453166841,1.59599685965665,1.53017908155183))
REPRESENTATION_ITEM('')
);
#524=(
BOUNDED_CURVE()
B_SPLINE_CURVE(2,(#30024,#30025,#30026),.UNSPECIFIED.,.F.,.F.)
B_SPLINE_CURVE_WITH_KNOTS((3,3),(-4.1476658994832,-3.45728242473689),
 .UNSPECIFIED.)
CURVE()
GEOMETRIC_REPRESENTATION_ITEM()
RATIONAL_B_SPLINE_CURVE((1.53018480461537,1.59600282888702,1.62522061017657))
REPRESENTATION_ITEM('')
);
#525=(
BOUNDED_CURVE()
B_SPLINE_CURVE(2,(#30027,#30028,#30029),.UNSPECIFIED.,.F.,.F.)
B_SPLINE_CURVE_WITH_KNOTS((3,3),(-2.35502343804527,-1.66463996329893),
 .UNSPECIFIED.)
CURVE()
GEOMETRIC_REPRESENTATION_ITEM()
RATIONAL_B_SPLINE_CURVE((1.62522061017658,1.59600282888702,1.53018480461537))
REPRESENTATION_ITEM('')
);
#526=(
BOUNDED_CURVE()
B_SPLINE_CURVE(2,(#30030,#30031,#30032),.UNSPECIFIED.,.F.,.F.)
B_SPLINE_CURVE_WITH_KNOTS((3,3),(-4.14763863034457,-3.45725829975024),
 .UNSPECIFIED.)
CURVE()
GEOMETRIC_REPRESENTATION_ITEM()
RATIONAL_B_SPLINE_CURVE((1.53017908155183,1.59599685965666,1.62521453166841))
REPRESENTATION_ITEM('')
);
#527=(
BOUNDED_CURVE()
B_SPLINE_CURVE(2,(#30033,#30034,#30035),.UNSPECIFIED.,.F.,.F.)
B_SPLINE_CURVE_WITH_KNOTS((3,3),(-2.35500433297853,-1.66462400238417),
 .UNSPECIFIED.)
CURVE()
GEOMETRIC_REPRESENTATION_ITEM()
RATIONAL_B_SPLINE_CURVE((1.62521453166842,1.59599685965666,1.53017908155183))
REPRESENTATION_ITEM('')
);
#528=(
BOUNDED_CURVE()
B_SPLINE_CURVE(2,(#30040,#30041,#30042),.UNSPECIFIED.,.F.,.F.)
B_SPLINE_CURVE_WITH_KNOTS((3,3),(-4.14766589948319,-3.45728242473685),
 .UNSPECIFIED.)
CURVE()
GEOMETRIC_REPRESENTATION_ITEM()
RATIONAL_B_SPLINE_CURVE((1.53018480461536,1.59600282888702,1.62522061017657))
REPRESENTATION_ITEM('')
);
#529=(
BOUNDED_CURVE()
B_SPLINE_CURVE(2,(#30043,#30044,#30045),.UNSPECIFIED.,.F.,.F.)
B_SPLINE_CURVE_WITH_KNOTS((3,3),(-2.35502343804525,-1.66463996329893),
 .UNSPECIFIED.)
CURVE()
GEOMETRIC_REPRESENTATION_ITEM()
RATIONAL_B_SPLINE_CURVE((1.62522061017657,1.59600282888702,1.53018480461537))
REPRESENTATION_ITEM('')
);
#530=(
BOUNDED_CURVE()
B_SPLINE_CURVE(2,(#30046,#30047,#30048),.UNSPECIFIED.,.F.,.F.)
B_SPLINE_CURVE_WITH_KNOTS((3,3),(-4.14763863034458,-3.45725829975023),
 .UNSPECIFIED.)
CURVE()
GEOMETRIC_REPRESENTATION_ITEM()
RATIONAL_B_SPLINE_CURVE((1.53017908155183,1.59599685965666,1.62521453166842))
REPRESENTATION_ITEM('')
);
#531=(
BOUNDED_CURVE()
B_SPLINE_CURVE(2,(#30049,#30050,#30051),.UNSPECIFIED.,.F.,.F.)
B_SPLINE_CURVE_WITH_KNOTS((3,3),(-2.35500433297852,-1.66462400238417),
 .UNSPECIFIED.)
CURVE()
GEOMETRIC_REPRESENTATION_ITEM()
RATIONAL_B_SPLINE_CURVE((1.62521453166842,1.59599685965666,1.53017908155183))
REPRESENTATION_ITEM('')
);
#532=(
BOUNDED_CURVE()
B_SPLINE_CURVE(2,(#30053,#30054,#30055),.UNSPECIFIED.,.F.,.F.)
B_SPLINE_CURVE_WITH_KNOTS((3,3),(-4.14765638055869,-3.45727400335153),
 .UNSPECIFIED.)
CURVE()
GEOMETRIC_REPRESENTATION_ITEM()
RATIONAL_B_SPLINE_CURVE((1.53018280684716,1.59600074518856,1.62521848833216))
REPRESENTATION_ITEM('')
);
#533=(
BOUNDED_CURVE()
B_SPLINE_CURVE(2,(#30056,#30057,#30058),.UNSPECIFIED.,.F.,.F.)
B_SPLINE_CURVE_WITH_KNOTS((3,3),(-2.35501676897951,-1.66463439177237),
 .UNSPECIFIED.)
CURVE()
GEOMETRIC_REPRESENTATION_ITEM()
RATIONAL_B_SPLINE_CURVE((1.62521848833216,1.59600074518856,1.53018280684716))
REPRESENTATION_ITEM('')
);
#534=(
BOUNDED_CURVE()
B_SPLINE_CURVE(2,(#30059,#30060,#30061),.UNSPECIFIED.,.F.,.F.)
B_SPLINE_CURVE_WITH_KNOTS((3,3),(-4.14763863034457,-3.45725829975022),
 .UNSPECIFIED.)
CURVE()
GEOMETRIC_REPRESENTATION_ITEM()
RATIONAL_B_SPLINE_CURVE((1.53017908155183,1.59599685965666,1.62521453166842))
REPRESENTATION_ITEM('')
);
#535=(
BOUNDED_CURVE()
B_SPLINE_CURVE(2,(#30062,#30063,#30064),.UNSPECIFIED.,.F.,.F.)
B_SPLINE_CURVE_WITH_KNOTS((3,3),(-2.35500433297853,-1.66462400238418),
 .UNSPECIFIED.)
CURVE()
GEOMETRIC_REPRESENTATION_ITEM()
RATIONAL_B_SPLINE_CURVE((1.62521453166842,1.59599685965666,1.53017908155183))
REPRESENTATION_ITEM('')
);
#536=(
BOUNDED_CURVE()
B_SPLINE_CURVE(2,(#30351,#30352,#30353,#30354,#30355,#30356,#30357,#30358,
#30359,#30360,#30361,#30362,#30363,#30364,#30365,#30366,#30367,#30368,#30369,
#30370,#30371),.UNSPECIFIED.,.F.,.F.)
B_SPLINE_CURVE_WITH_KNOTS((3,2,2,2,2,2,2,2,2,2,3),(0.214285714285714,0.228571428571429,
0.242857142857143,0.257142857142857,0.271428571428571,0.285714285714286,
0.3,0.314285714285714,0.328571428571429,0.342857142857143,0.357142857142857),
 .UNSPECIFIED.)
CURVE()
GEOMETRIC_REPRESENTATION_ITEM()
RATIONAL_B_SPLINE_CURVE((1.,0.951056516295154,1.,0.951056516295154,1.,0.951056516295154,
1.,0.951056516295154,1.,0.951056516295154,1.,0.951056516295154,1.,0.951056516295154,
1.,0.951056516295154,1.,0.951056516295154,1.,0.951056516295154,1.))
REPRESENTATION_ITEM('')
);
#537=(
BOUNDED_CURVE()
B_SPLINE_CURVE(2,(#30373,#30374,#30375,#30376,#30377,#30378,#30379,#30380,
#30381,#30382,#30383,#30384,#30385,#30386,#30387,#30388,#30389,#30390,#30391,
#30392,#30393),.UNSPECIFIED.,.F.,.F.)
B_SPLINE_CURVE_WITH_KNOTS((3,2,2,2,2,2,2,2,2,2,3),(0.222802766307425,0.237656284061254,
0.252509801815083,0.267363319568912,0.282216837322741,0.29707035507657,
0.311923872830398,0.326777390584227,0.341630908338056,0.356484426091885,
0.371337943845714),.UNSPECIFIED.)
CURVE()
GEOMETRIC_REPRESENTATION_ITEM()
RATIONAL_B_SPLINE_CURVE((1.,0.951056516295154,1.,0.951056516295154,1.,0.951056516295154,
1.,0.951056516295154,1.,0.951056516295154,1.,0.951056516295154,1.,0.951056516295154,
1.,0.951056516295154,1.,0.951056516295154,1.,0.951056516295154,1.))
REPRESENTATION_ITEM('')
);
#538=(
BOUNDED_CURVE()
B_SPLINE_CURVE(2,(#32588,#32589,#32590),.UNSPECIFIED.,.F.,.F.)
B_SPLINE_CURVE_WITH_KNOTS((3,3),(-3.03150105849453,-1.74744567255227),
 .UNSPECIFIED.)
CURVE()
GEOMETRIC_REPRESENTATION_ITEM()
RATIONAL_B_SPLINE_CURVE((1.66716031106357,1.66716031106357,1.54746358611627))
REPRESENTATION_ITEM('')
);
#539=(
BOUNDED_CURVE()
B_SPLINE_CURVE(2,(#32591,#32592,#32593),.UNSPECIFIED.,.F.,.F.)
B_SPLINE_CURVE_WITH_KNOTS((3,3),(-4.3155564444368,-3.03150105849454),
 .UNSPECIFIED.)
CURVE()
GEOMETRIC_REPRESENTATION_ITEM()
RATIONAL_B_SPLINE_CURVE((1.54746358611627,1.66716031106357,1.66716031106357))
REPRESENTATION_ITEM('')
);
#540=(
BOUNDED_CURVE()
B_SPLINE_CURVE(2,(#32596,#32597,#32598),.UNSPECIFIED.,.F.,.F.)
B_SPLINE_CURVE_WITH_KNOTS((3,3),(-3.03150105849453,-1.74744567255227),
 .UNSPECIFIED.)
CURVE()
GEOMETRIC_REPRESENTATION_ITEM()
RATIONAL_B_SPLINE_CURVE((1.66716031106357,1.66716031106357,1.54746358611627))
REPRESENTATION_ITEM('')
);
#541=(
BOUNDED_CURVE()
B_SPLINE_CURVE(2,(#32599,#32600,#32601),.UNSPECIFIED.,.F.,.F.)
B_SPLINE_CURVE_WITH_KNOTS((3,3),(-4.31555644443679,-3.03150105849453),
 .UNSPECIFIED.)
CURVE()
GEOMETRIC_REPRESENTATION_ITEM()
RATIONAL_B_SPLINE_CURVE((1.54746358611627,1.66716031106357,1.66716031106357))
REPRESENTATION_ITEM('')
);
#542=(
BOUNDED_CURVE()
B_SPLINE_CURVE(2,(#32604,#32605,#32606),.UNSPECIFIED.,.F.,.F.)
B_SPLINE_CURVE_WITH_KNOTS((3,3),(-4.3155564444368,-3.03150105849453),
 .UNSPECIFIED.)
CURVE()
GEOMETRIC_REPRESENTATION_ITEM()
RATIONAL_B_SPLINE_CURVE((1.54746358611627,1.66716031106357,1.66716031106357))
REPRESENTATION_ITEM('')
);
#543=(
BOUNDED_CURVE()
B_SPLINE_CURVE(2,(#32607,#32608,#32609),.UNSPECIFIED.,.F.,.F.)
B_SPLINE_CURVE_WITH_KNOTS((3,3),(-3.03150105849453,-1.74744567255227),
 .UNSPECIFIED.)
CURVE()
GEOMETRIC_REPRESENTATION_ITEM()
RATIONAL_B_SPLINE_CURVE((1.66716031106357,1.66716031106357,1.54746358611627))
REPRESENTATION_ITEM('')
);
#544=(
BOUNDED_CURVE()
B_SPLINE_CURVE(2,(#32612,#32613,#32614),.UNSPECIFIED.,.F.,.F.)
B_SPLINE_CURVE_WITH_KNOTS((3,3),(-4.3155564444368,-3.03150105849453),
 .UNSPECIFIED.)
CURVE()
GEOMETRIC_REPRESENTATION_ITEM()
RATIONAL_B_SPLINE_CURVE((1.54746358611627,1.66716031106357,1.66716031106357))
REPRESENTATION_ITEM('')
);
#545=(
BOUNDED_CURVE()
B_SPLINE_CURVE(2,(#32615,#32616,#32617),.UNSPECIFIED.,.F.,.F.)
B_SPLINE_CURVE_WITH_KNOTS((3,3),(-3.03150105849453,-1.74744567255227),
 .UNSPECIFIED.)
CURVE()
GEOMETRIC_REPRESENTATION_ITEM()
RATIONAL_B_SPLINE_CURVE((1.66716031106357,1.66716031106357,1.54746358611627))
REPRESENTATION_ITEM('')
);
#546=(
BOUNDED_CURVE()
B_SPLINE_CURVE(2,(#32620,#32621,#32622),.UNSPECIFIED.,.F.,.F.)
B_SPLINE_CURVE_WITH_KNOTS((3,3),(-3.03150105849454,-1.74744567255227),
 .UNSPECIFIED.)
CURVE()
GEOMETRIC_REPRESENTATION_ITEM()
RATIONAL_B_SPLINE_CURVE((1.66716031106357,1.66716031106357,1.54746358611627))
REPRESENTATION_ITEM('')
);
#547=(
BOUNDED_CURVE()
B_SPLINE_CURVE(2,(#32623,#32624,#32625),.UNSPECIFIED.,.F.,.F.)
B_SPLINE_CURVE_WITH_KNOTS((3,3),(-4.3155564444368,-3.03150105849454),
 .UNSPECIFIED.)
CURVE()
GEOMETRIC_REPRESENTATION_ITEM()
RATIONAL_B_SPLINE_CURVE((1.54746358611627,1.66716031106357,1.66716031106357))
REPRESENTATION_ITEM('')
);
#548=(
BOUNDED_CURVE()
B_SPLINE_CURVE(2,(#32628,#32629,#32630),.UNSPECIFIED.,.F.,.F.)
B_SPLINE_CURVE_WITH_KNOTS((3,3),(-4.3155564444368,-3.03150105849453),
 .UNSPECIFIED.)
CURVE()
GEOMETRIC_REPRESENTATION_ITEM()
RATIONAL_B_SPLINE_CURVE((1.54746358611627,1.66716031106357,1.66716031106357))
REPRESENTATION_ITEM('')
);
#549=(
BOUNDED_CURVE()
B_SPLINE_CURVE(2,(#32631,#32632,#32633),.UNSPECIFIED.,.F.,.F.)
B_SPLINE_CURVE_WITH_KNOTS((3,3),(-3.03150105849454,-1.74744567255227),
 .UNSPECIFIED.)
CURVE()
GEOMETRIC_REPRESENTATION_ITEM()
RATIONAL_B_SPLINE_CURVE((1.66716031106357,1.66716031106357,1.54746358611627))
REPRESENTATION_ITEM('')
);
#550=(
BOUNDED_CURVE()
B_SPLINE_CURVE(2,(#32689,#32690,#32691),.UNSPECIFIED.,.F.,.F.)
B_SPLINE_CURVE_WITH_KNOTS((3,3),(2.31550755136326,3.79303994872323),
 .UNSPECIFIED.)
CURVE()
GEOMETRIC_REPRESENTATION_ITEM()
RATIONAL_B_SPLINE_CURVE((1.76182294006033,1.89810041873942,1.89810041873942))
REPRESENTATION_ITEM('')
);
#551=(
BOUNDED_CURVE()
B_SPLINE_CURVE(2,(#32693,#32694,#32695),.UNSPECIFIED.,.F.,.F.)
B_SPLINE_CURVE_WITH_KNOTS((3,3),(3.79303994872323,5.27057234608321),
 .UNSPECIFIED.)
CURVE()
GEOMETRIC_REPRESENTATION_ITEM()
RATIONAL_B_SPLINE_CURVE((1.89810041873942,1.89810041873942,1.76182294006033))
REPRESENTATION_ITEM('')
);
#552=(
BOUNDED_CURVE()
B_SPLINE_CURVE(2,(#32699,#32700,#32701),.UNSPECIFIED.,.F.,.F.)
B_SPLINE_CURVE_WITH_KNOTS((3,3),(-3.79303994872324,-2.31550755136325),
 .UNSPECIFIED.)
CURVE()
GEOMETRIC_REPRESENTATION_ITEM()
RATIONAL_B_SPLINE_CURVE((1.89810041873942,1.89810041873942,1.76182294006033))
REPRESENTATION_ITEM('')
);
#553=(
BOUNDED_CURVE()
B_SPLINE_CURVE(2,(#32702,#32703,#32704),.UNSPECIFIED.,.F.,.F.)
B_SPLINE_CURVE_WITH_KNOTS((3,3),(-5.27057234608319,-3.79303994872324),
 .UNSPECIFIED.)
CURVE()
GEOMETRIC_REPRESENTATION_ITEM()
RATIONAL_B_SPLINE_CURVE((1.76182294006033,1.89810041873942,1.89810041873942))
REPRESENTATION_ITEM('')
);
#554=(
BOUNDED_CURVE()
B_SPLINE_CURVE(2,(#32707,#32708,#32709),.UNSPECIFIED.,.F.,.F.)
B_SPLINE_CURVE_WITH_KNOTS((3,3),(2.31550755136325,3.79303994872323),
 .UNSPECIFIED.)
CURVE()
GEOMETRIC_REPRESENTATION_ITEM()
RATIONAL_B_SPLINE_CURVE((1.76182294006033,1.89810041873942,1.89810041873942))
REPRESENTATION_ITEM('')
);
#555=(
BOUNDED_CURVE()
B_SPLINE_CURVE(2,(#32711,#32712,#32713),.UNSPECIFIED.,.F.,.F.)
B_SPLINE_CURVE_WITH_KNOTS((3,3),(3.79303994872323,5.27057234608319),
 .UNSPECIFIED.)
CURVE()
GEOMETRIC_REPRESENTATION_ITEM()
RATIONAL_B_SPLINE_CURVE((1.89810041873942,1.89810041873941,1.76182294006033))
REPRESENTATION_ITEM('')
);
#556=(
BOUNDED_CURVE()
B_SPLINE_CURVE(2,(#32717,#32718,#32719),.UNSPECIFIED.,.F.,.F.)
B_SPLINE_CURVE_WITH_KNOTS((3,3),(-3.79303994872322,-2.31550755136326),
 .UNSPECIFIED.)
CURVE()
GEOMETRIC_REPRESENTATION_ITEM()
RATIONAL_B_SPLINE_CURVE((1.89810041873942,1.89810041873942,1.76182294006033))
REPRESENTATION_ITEM('')
);
#557=(
BOUNDED_CURVE()
B_SPLINE_CURVE(2,(#32720,#32721,#32722),.UNSPECIFIED.,.F.,.F.)
B_SPLINE_CURVE_WITH_KNOTS((3,3),(-5.27057234608319,-3.79303994872322),
 .UNSPECIFIED.)
CURVE()
GEOMETRIC_REPRESENTATION_ITEM()
RATIONAL_B_SPLINE_CURVE((1.76182294006033,1.89810041873942,1.89810041873942))
REPRESENTATION_ITEM('')
);
#558=(
BOUNDED_CURVE()
B_SPLINE_CURVE(2,(#32726,#32727,#32728),.UNSPECIFIED.,.F.,.F.)
B_SPLINE_CURVE_WITH_KNOTS((3,3),(2.31550755136325,3.79303994872322),
 .UNSPECIFIED.)
CURVE()
GEOMETRIC_REPRESENTATION_ITEM()
RATIONAL_B_SPLINE_CURVE((1.76182294006033,1.89810041873941,1.89810041873941))
REPRESENTATION_ITEM('')
);
#559=(
BOUNDED_CURVE()
B_SPLINE_CURVE(2,(#32732,#32733,#32734),.UNSPECIFIED.,.F.,.F.)
B_SPLINE_CURVE_WITH_KNOTS((3,3),(-5.27057234608321,-3.79303994872322),
 .UNSPECIFIED.)
CURVE()
GEOMETRIC_REPRESENTATION_ITEM()
RATIONAL_B_SPLINE_CURVE((1.76182294006033,1.89810041873941,1.89810041873941))
REPRESENTATION_ITEM('')
);
#560=(
BOUNDED_CURVE()
B_SPLINE_CURVE(2,(#32735,#32736,#32737),.UNSPECIFIED.,.F.,.F.)
B_SPLINE_CURVE_WITH_KNOTS((3,3),(-3.79303994872322,-2.31550755136325),
 .UNSPECIFIED.)
CURVE()
GEOMETRIC_REPRESENTATION_ITEM()
RATIONAL_B_SPLINE_CURVE((1.89810041873941,1.89810041873941,1.76182294006033))
REPRESENTATION_ITEM('')
);
#561=(
BOUNDED_CURVE()
B_SPLINE_CURVE(2,(#32738,#32739,#32740),.UNSPECIFIED.,.F.,.F.)
B_SPLINE_CURVE_WITH_KNOTS((3,3),(3.79303994872322,5.2705723460832),
 .UNSPECIFIED.)
CURVE()
GEOMETRIC_REPRESENTATION_ITEM()
RATIONAL_B_SPLINE_CURVE((1.89810041873941,1.89810041873941,1.76182294006033))
REPRESENTATION_ITEM('')
);
#562=(
BOUNDED_CURVE()
B_SPLINE_CURVE(2,(#32743,#32744,#32745),.UNSPECIFIED.,.F.,.F.)
B_SPLINE_CURVE_WITH_KNOTS((3,3),(2.31550755136326,3.79303994872322),
 .UNSPECIFIED.)
CURVE()
GEOMETRIC_REPRESENTATION_ITEM()
RATIONAL_B_SPLINE_CURVE((1.76182294006033,1.89810041873941,1.89810041873941))
REPRESENTATION_ITEM('')
);
#563=(
BOUNDED_CURVE()
B_SPLINE_CURVE(2,(#32747,#32748,#32749),.UNSPECIFIED.,.F.,.F.)
B_SPLINE_CURVE_WITH_KNOTS((3,3),(3.79303994872322,5.2705723460832),
 .UNSPECIFIED.)
CURVE()
GEOMETRIC_REPRESENTATION_ITEM()
RATIONAL_B_SPLINE_CURVE((1.89810041873941,1.89810041873941,1.76182294006033))
REPRESENTATION_ITEM('')
);
#564=(
BOUNDED_CURVE()
B_SPLINE_CURVE(2,(#32753,#32754,#32755),.UNSPECIFIED.,.F.,.F.)
B_SPLINE_CURVE_WITH_KNOTS((3,3),(-3.79303994872323,-2.31550755136325),
 .UNSPECIFIED.)
CURVE()
GEOMETRIC_REPRESENTATION_ITEM()
RATIONAL_B_SPLINE_CURVE((1.89810041873941,1.89810041873941,1.76182294006033))
REPRESENTATION_ITEM('')
);
#565=(
BOUNDED_CURVE()
B_SPLINE_CURVE(2,(#32756,#32757,#32758),.UNSPECIFIED.,.F.,.F.)
B_SPLINE_CURVE_WITH_KNOTS((3,3),(-5.27057234608319,-3.79303994872323),
 .UNSPECIFIED.)
CURVE()
GEOMETRIC_REPRESENTATION_ITEM()
RATIONAL_B_SPLINE_CURVE((1.76182294006033,1.89810041873941,1.89810041873941))
REPRESENTATION_ITEM('')
);
#566=(
BOUNDED_CURVE()
B_SPLINE_CURVE(2,(#32761,#32762,#32763),.UNSPECIFIED.,.F.,.F.)
B_SPLINE_CURVE_WITH_KNOTS((3,3),(2.31550755136326,3.79303994872322),
 .UNSPECIFIED.)
CURVE()
GEOMETRIC_REPRESENTATION_ITEM()
RATIONAL_B_SPLINE_CURVE((1.76182294006033,1.89810041873941,1.89810041873941))
REPRESENTATION_ITEM('')
);
#567=(
BOUNDED_CURVE()
B_SPLINE_CURVE(2,(#32765,#32766,#32767),.UNSPECIFIED.,.F.,.F.)
B_SPLINE_CURVE_WITH_KNOTS((3,3),(3.79303994872322,5.27057234608318),
 .UNSPECIFIED.)
CURVE()
GEOMETRIC_REPRESENTATION_ITEM()
RATIONAL_B_SPLINE_CURVE((1.89810041873941,1.89810041873941,1.76182294006033))
REPRESENTATION_ITEM('')
);
#568=(
BOUNDED_CURVE()
B_SPLINE_CURVE(2,(#32771,#32772,#32773),.UNSPECIFIED.,.F.,.F.)
B_SPLINE_CURVE_WITH_KNOTS((3,3),(-3.79303994872322,-2.31550755136326),
 .UNSPECIFIED.)
CURVE()
GEOMETRIC_REPRESENTATION_ITEM()
RATIONAL_B_SPLINE_CURVE((1.89810041873941,1.89810041873941,1.76182294006033))
REPRESENTATION_ITEM('')
);
#569=(
BOUNDED_CURVE()
B_SPLINE_CURVE(2,(#32774,#32775,#32776),.UNSPECIFIED.,.F.,.F.)
B_SPLINE_CURVE_WITH_KNOTS((3,3),(-5.27057234608318,-3.79303994872322),
 .UNSPECIFIED.)
CURVE()
GEOMETRIC_REPRESENTATION_ITEM()
RATIONAL_B_SPLINE_CURVE((1.76182294006033,1.89810041873941,1.89810041873941))
REPRESENTATION_ITEM('')
);
#570=(
BOUNDED_CURVE()
B_SPLINE_CURVE(2,(#32779,#32780,#32781),.UNSPECIFIED.,.F.,.F.)
B_SPLINE_CURVE_WITH_KNOTS((3,3),(2.31550755136325,3.79303994872323),
 .UNSPECIFIED.)
CURVE()
GEOMETRIC_REPRESENTATION_ITEM()
RATIONAL_B_SPLINE_CURVE((1.76182294006033,1.89810041873942,1.89810041873942))
REPRESENTATION_ITEM('')
);
#571=(
BOUNDED_CURVE()
B_SPLINE_CURVE(2,(#32782,#32783,#32784),.UNSPECIFIED.,.F.,.F.)
B_SPLINE_CURVE_WITH_KNOTS((3,3),(3.79303994872323,5.27057234608319),
 .UNSPECIFIED.)
CURVE()
GEOMETRIC_REPRESENTATION_ITEM()
RATIONAL_B_SPLINE_CURVE((1.89810041873942,1.89810041873942,1.76182294006033))
REPRESENTATION_ITEM('')
);
#572=(
BOUNDED_CURVE()
B_SPLINE_CURVE(2,(#32786,#32787,#32788),.UNSPECIFIED.,.F.,.F.)
B_SPLINE_CURVE_WITH_KNOTS((3,3),(-3.79303994872322,-2.31550755136325),
 .UNSPECIFIED.)
CURVE()
GEOMETRIC_REPRESENTATION_ITEM()
RATIONAL_B_SPLINE_CURVE((1.89810041873942,1.89810041873942,1.76182294006033))
REPRESENTATION_ITEM('')
);
#573=(
BOUNDED_CURVE()
B_SPLINE_CURVE(2,(#32789,#32790,#32791),.UNSPECIFIED.,.F.,.F.)
B_SPLINE_CURVE_WITH_KNOTS((3,3),(-5.2705723460832,-3.79303994872322),
 .UNSPECIFIED.)
CURVE()
GEOMETRIC_REPRESENTATION_ITEM()
RATIONAL_B_SPLINE_CURVE((1.76182294006033,1.89810041873942,1.89810041873942))
REPRESENTATION_ITEM('')
);
#574=CONICAL_SURFACE('',#16277,7.09803,0.785398163397448);
#575=CONICAL_SURFACE('',#16290,13.4874,1.0471975511966);
#576=CONICAL_SURFACE('',#16292,13.4874,1.0471975511966);
#577=CONICAL_SURFACE('',#16294,13.4874,1.0471975511966);
#578=CONICAL_SURFACE('',#16296,13.4874,1.0471975511966);
#579=CONICAL_SURFACE('',#16298,13.4874,1.0471975511966);
#580=CONICAL_SURFACE('',#16300,13.4874,1.0471975511966);
#581=CONICAL_SURFACE('',#16304,7.09803,0.785398163397444);
#582=CONICAL_SURFACE('',#16317,13.4874,1.0471975511966);
#583=CONICAL_SURFACE('',#16319,13.4874,1.0471975511966);
#584=CONICAL_SURFACE('',#16321,13.4874,1.0471975511966);
#585=CONICAL_SURFACE('',#16323,13.4874,1.0471975511966);
#586=CONICAL_SURFACE('',#16325,13.4874,1.0471975511966);
#587=CONICAL_SURFACE('',#16327,13.4874,1.0471975511966);
#588=CONICAL_SURFACE('',#16335,7.9375,0.959931088596874);
#589=CONICAL_SURFACE('',#16338,7.282307,0.959931088596874);
#590=CONICAL_SURFACE('',#16362,11.9126,0.859709158487534);
#591=CONICAL_SURFACE('',#16363,11.9126,0.859709158487534);
#592=CONICAL_SURFACE('',#16364,11.9126,0.859709158487534);
#593=CONICAL_SURFACE('',#16365,11.9126,0.859709158487534);
#594=CONICAL_SURFACE('',#16366,11.9126,0.859709158487534);
#595=CONICAL_SURFACE('',#16367,11.9126,0.859709158487534);
#596=CONICAL_SURFACE('',#16368,11.9126,0.859709158487534);
#597=CONICAL_SURFACE('',#16369,11.9126,0.859709158487534);
#598=CONICAL_SURFACE('',#16370,11.9126,0.859709158487534);
#599=CONICAL_SURFACE('',#16371,11.9126,0.859709158487534);
#600=CONICAL_SURFACE('',#16372,11.9126,0.859709158487534);
#601=CONICAL_SURFACE('',#16373,11.9126,0.859709158487534);
#602=CONICAL_SURFACE('',#16434,4.93749999999999,0.785398163397446);
#603=CONICAL_SURFACE('',#16468,4.93749999999997,0.785398163397445);
#604=CONICAL_SURFACE('',#16474,7.9375,0.785398163397451);
#605=CONICAL_SURFACE('',#16480,12.246709909405,0.785398163397453);
#606=CONICAL_SURFACE('',#16504,13.746709909405,0.785398163397448);
#607=CONICAL_SURFACE('',#16505,13.746709909405,0.785398163397448);
#608=CONICAL_SURFACE('',#16506,12.246709909405,0.785398163397453);
#609=CONICAL_SURFACE('',#16507,12.246709909405,0.785398163397453);
#610=CONICAL_SURFACE('',#16508,13.746709909405,0.785398163397448);
#611=CONICAL_SURFACE('',#16509,12.246709909405,0.785398163397453);
#612=CONICAL_SURFACE('',#16510,13.746709909405,0.785398163397448);
#613=CONICAL_SURFACE('',#16511,12.246709909405,0.785398163397453);
#614=CONICAL_SURFACE('',#16512,13.746709909405,0.785398163397448);
#615=CONICAL_SURFACE('',#16513,12.246709909405,0.785398163397453);
#616=CONICAL_SURFACE('',#16514,13.746709909405,0.785398163397448);
#617=CONICAL_SURFACE('',#16515,12.246709909405,0.785398163397453);
#618=CONICAL_SURFACE('',#17021,6.8985,0.785398163397446);
#619=CONICAL_SURFACE('',#17040,13.5,1.0471975511966);
#620=CONICAL_SURFACE('',#17041,13.5,1.0471975511966);
#621=CONICAL_SURFACE('',#17042,13.5,1.0471975511966);
#622=CONICAL_SURFACE('',#17043,13.5,1.0471975511966);
#623=CONICAL_SURFACE('',#17044,13.5,1.0471975511966);
#624=CONICAL_SURFACE('',#17045,13.5,1.0471975511966);
#625=CONICAL_SURFACE('',#17066,8.,0.95993108859688);
#626=CONICAL_SURFACE('',#17069,6.9,0.95993108859688);
#627=CONICAL_SURFACE('',#17093,13.5,1.0471975511966);
#628=CONICAL_SURFACE('',#17094,13.5,1.0471975511966);
#629=CONICAL_SURFACE('',#17095,13.5,1.0471975511966);
#630=CONICAL_SURFACE('',#17096,13.5,1.0471975511966);
#631=CONICAL_SURFACE('',#17097,13.5,1.0471975511966);
#632=CONICAL_SURFACE('',#17098,13.5,1.0471975511966);
#633=CONICAL_SURFACE('',#17099,13.5,1.0471975511966);
#634=CONICAL_SURFACE('',#17100,13.5,1.0471975511966);
#635=CONICAL_SURFACE('',#17101,13.5,1.0471975511966);
#636=CONICAL_SURFACE('',#17102,13.5,1.0471975511966);
#637=CONICAL_SURFACE('',#17103,13.5,1.0471975511966);
#638=CONICAL_SURFACE('',#17104,13.5,1.0471975511966);
#639=TOROIDAL_SURFACE('',#16259,11.,7.93749999999998);
#640=TOROIDAL_SURFACE('',#16264,11.,7.93749999999998);
#641=TOROIDAL_SURFACE('',#16420,15.,3.);
#642=TOROIDAL_SURFACE('',#16425,15.,3.);
#643=TOROIDAL_SURFACE('',#17008,9.2,1.2);
#644=ELLIPSE('',#16043,10.9424774388658,7.73750000000281);
#645=ELLIPSE('',#16044,11.2253201513379,7.93750000000103);
#646=ELLIPSE('',#16045,10.9424774388637,7.73750000000177);
#647=ELLIPSE('',#16047,10.9424774388587,7.73749999999781);
#648=ELLIPSE('',#16048,11.2253201513381,7.93750000000136);
#649=ELLIPSE('',#16049,10.9424774388615,7.73749999999964);
#650=ELLIPSE('',#16060,10.9424774388615,7.73749999999999);
#651=ELLIPSE('',#16061,11.2253201513371,7.93750000000052);
#652=ELLIPSE('',#16062,10.9424774388621,7.73750000000035);
#653=ELLIPSE('',#16064,10.9424774388604,7.73749999999896);
#654=ELLIPSE('',#16065,11.2253201513326,7.93749999999674);
#655=ELLIPSE('',#16066,10.9424774388621,7.73750000000041);
#656=ELLIPSE('',#16077,10.9424774388579,7.73749999999704);
#657=ELLIPSE('',#16078,11.2253201513353,7.9374999999993);
#658=ELLIPSE('',#16079,10.9424774388611,7.73749999999964);
#659=ELLIPSE('',#16081,10.9424774388619,7.73750000000076);
#660=ELLIPSE('',#16082,11.2253201513349,7.93749999999867);
#661=ELLIPSE('',#16083,10.942477438863,7.73750000000083);
#662=ELLIPSE('',#16160,10.9424774388598,7.7374999999982);
#663=ELLIPSE('',#16164,10.9424774388633,7.73750000000104);
#664=ELLIPSE('',#16165,11.225320151339,7.9375000000018);
#665=ELLIPSE('',#16166,10.9424774388576,7.73749999999669);
#666=ELLIPSE('',#16168,10.9424774388584,7.73749999999717);
#667=ELLIPSE('',#16169,11.2253201513371,7.93750000000039);
#668=ELLIPSE('',#16476,29.6250000052051,10.4740191977281);
#669=ELLIPSE('',#16477,29.6250000012,10.4740191966556);
#670=ELLIPSE('',#16483,6.58333333333336,4.93750000000003);
#671=ELLIPSE('',#16485,6.58333333333341,4.93750000000007);
#672=SHAPE_REPRESENTATION_RELATIONSHIP('SRR','None',#33013,#686);
#673=SHAPE_REPRESENTATION_RELATIONSHIP('SRR','None',#33014,#687);
#674=SHAPE_REPRESENTATION_RELATIONSHIP('SRR','None',#33016,#688);
#675=SHAPE_REPRESENTATION_RELATIONSHIP('SRR','None',#33017,#689);
#676=SHAPE_REPRESENTATION_RELATIONSHIP('SRR','None',#33018,#690);
#677=SHAPE_REPRESENTATION_RELATIONSHIP('SRR','None',#33019,#691);
#678=SHAPE_REPRESENTATION_RELATIONSHIP('SRR','None',#33020,#692);
#679=SHAPE_REPRESENTATION_RELATIONSHIP('SRR','None',#33021,#693);
#680=SHAPE_REPRESENTATION_RELATIONSHIP('SRR','None',#33022,#694);
#681=SHAPE_REPRESENTATION_RELATIONSHIP('SRR','None',#33023,#695);
#682=SHAPE_REPRESENTATION_RELATIONSHIP('SRR','None',#33024,#696);
#683=SHAPE_REPRESENTATION_RELATIONSHIP('SRR','None',#33025,#697);
#684=SHAPE_REPRESENTATION_RELATIONSHIP('SRR','None',#33026,#698);
#685=SHAPE_REPRESENTATION_RELATIONSHIP('SRR','None',#33027,#699);
#686=ADVANCED_BREP_SHAPE_REPRESENTATION('',(#1380,#1381,#1382,#1383,#1384,
#1385,#1386,#1387,#1388),#32888);
#687=ADVANCED_BREP_SHAPE_REPRESENTATION('',(#1389,#1390,#1391,#1392,#1393),
#32889);
#688=ADVANCED_BREP_SHAPE_REPRESENTATION('',(#1394,#1395,#1396,#1397,#1398,
#1399,#1400,#1401,#1402,#1403),#32891);
#689=ADVANCED_BREP_SHAPE_REPRESENTATION('',(#1404,#1405,#1406,#1407),#32892);
#690=ADVANCED_BREP_SHAPE_REPRESENTATION('',(#1408),#32893);
#691=ADVANCED_BREP_SHAPE_REPRESENTATION('',(#1409),#32894);
#692=ADVANCED_BREP_SHAPE_REPRESENTATION('',(#1410),#32895);
#693=ADVANCED_BREP_SHAPE_REPRESENTATION('',(#1411),#32896);
#694=ADVANCED_BREP_SHAPE_REPRESENTATION('',(#1412),#32897);
#695=ADVANCED_BREP_SHAPE_REPRESENTATION('',(#1413),#32898);
#696=ADVANCED_BREP_SHAPE_REPRESENTATION('',(#1414,#1415,#1416,#1417,#1418,
#1419,#1420,#1421,#1422,#1423,#1424,#1425,#1426,#1427,#1428,#1429,#1430,
#1431,#1432,#1433,#1434,#1435,#1436,#1437,#1438,#1439,#1440,#1441,#1442,
#1443,#1444,#1445,#1446,#1447,#1448,#1449,#1450,#1451,#1452,#1453,#1454,
#1455,#1456,#1457,#1458,#1459,#1460,#1461,#1462,#1463,#1464,#1465),#32899);
#697=ADVANCED_BREP_SHAPE_REPRESENTATION('',(#1466),#32900);
#698=ADVANCED_BREP_SHAPE_REPRESENTATION('',(#1467),#32901);
#699=ADVANCED_BREP_SHAPE_REPRESENTATION('',(#1468),#32902);
#700=CIRCLE('',#15798,75.0000000000001);
#701=CIRCLE('',#15799,75.0000000000001);
#702=CIRCLE('',#15808,75.0000000000001);
#703=CIRCLE('',#15809,75.0000000000001);
#704=CIRCLE('',#15816,8.99999999999998);
#705=CIRCLE('',#15817,8.99999999999998);
#706=CIRCLE('',#15819,8.99999999999998);
#707=CIRCLE('',#15820,8.99999999999998);
#708=CIRCLE('',#15822,8.99999999999998);
#709=CIRCLE('',#15823,8.99999999999998);
#710=CIRCLE('',#15825,8.99999999999998);
#711=CIRCLE('',#15826,8.99999999999998);
#712=CIRCLE('',#15828,8.99999999999998);
#713=CIRCLE('',#15829,8.99999999999998);
#714=CIRCLE('',#15831,8.99999999999998);
#715=CIRCLE('',#15832,8.99999999999998);
#716=CIRCLE('',#15840,8.99999999999998);
#717=CIRCLE('',#15841,8.99999999999998);
#718=CIRCLE('',#15843,9.00000000000001);
#719=CIRCLE('',#15844,9.00000000000001);
#720=CIRCLE('',#15846,9.00000000000001);
#721=CIRCLE('',#15847,9.00000000000001);
#722=CIRCLE('',#15849,9.00000000000001);
#723=CIRCLE('',#15850,9.00000000000001);
#724=CIRCLE('',#15852,9.00000000000001);
#725=CIRCLE('',#15853,9.00000000000001);
#726=CIRCLE('',#15861,8.99999999999998);
#727=CIRCLE('',#15862,8.99999999999998);
#728=CIRCLE('',#15864,9.00000000000001);
#729=CIRCLE('',#15865,9.00000000000001);
#730=CIRCLE('',#15867,9.00000000000001);
#731=CIRCLE('',#15868,9.00000000000001);
#732=CIRCLE('',#15870,9.00000000000001);
#733=CIRCLE('',#15871,9.00000000000001);
#734=CIRCLE('',#15873,9.00000000000001);
#735=CIRCLE('',#15874,9.00000000000001);
#736=CIRCLE('',#15901,9.00000000000006);
#737=CIRCLE('',#15902,9.00000000000006);
#738=CIRCLE('',#15904,9.00000000000006);
#739=CIRCLE('',#15905,9.00000000000006);
#740=CIRCLE('',#15907,9.00000000000005);
#741=CIRCLE('',#15908,9.00000000000005);
#742=CIRCLE('',#15910,9.00000000000005);
#743=CIRCLE('',#15911,9.00000000000005);
#744=CIRCLE('',#15913,9.00000000000006);
#745=CIRCLE('',#15914,9.00000000000006);
#746=CIRCLE('',#15916,9.00000000000006);
#747=CIRCLE('',#15917,9.00000000000006);
#748=CIRCLE('',#15919,9.00000000000006);
#749=CIRCLE('',#15920,9.00000000000006);
#750=CIRCLE('',#15922,9.00000000000006);
#751=CIRCLE('',#15923,9.00000000000006);
#752=CIRCLE('',#15925,9.00000000000006);
#753=CIRCLE('',#15926,9.00000000000006);
#754=CIRCLE('',#15928,9.00000000000006);
#755=CIRCLE('',#15929,9.00000000000006);
#756=CIRCLE('',#15931,9.00000000000406);
#757=CIRCLE('',#15932,9.00000000000406);
#758=CIRCLE('',#15934,9.00000000000006);
#759=CIRCLE('',#15935,9.00000000000006);
#760=CIRCLE('',#15937,9.00000000000006);
#761=CIRCLE('',#15938,9.00000000000006);
#762=CIRCLE('',#15940,9.00000000000006);
#763=CIRCLE('',#15941,9.00000000000006);
#764=CIRCLE('',#15943,9.00000000000006);
#765=CIRCLE('',#15944,9.00000000000006);
#766=CIRCLE('',#15946,31.0000000000001);
#767=CIRCLE('',#15947,31.0000000000001);
#768=CIRCLE('',#15949,138.);
#769=CIRCLE('',#15950,138.);
#770=CIRCLE('',#15952,9.00000000000006);
#771=CIRCLE('',#15953,9.00000000000006);
#772=CIRCLE('',#15961,136.525);
#773=CIRCLE('',#15962,136.525);
#774=CIRCLE('',#15964,121.435);
#775=CIRCLE('',#15965,121.435);
#776=CIRCLE('',#15969,30.165);
#777=CIRCLE('',#15970,30.165);
#778=CIRCLE('',#15972,26.255);
#779=CIRCLE('',#15973,26.255);
#780=CIRCLE('',#15977,12.4999999999953);
#781=CIRCLE('',#15978,12.4999999999953);
#782=CIRCLE('',#15980,12.4999999999835);
#783=CIRCLE('',#15981,12.4999999999835);
#784=CIRCLE('',#15983,12.4999999999698);
#785=CIRCLE('',#15984,12.4999999999698);
#786=CIRCLE('',#15986,12.4999999999583);
#787=CIRCLE('',#15987,12.4999999999583);
#788=CIRCLE('',#15989,12.4999999999518);
#789=CIRCLE('',#15990,12.4999999999518);
#790=CIRCLE('',#15992,12.4999999999521);
#791=CIRCLE('',#15993,12.4999999999521);
#792=CIRCLE('',#15995,12.499999999959);
#793=CIRCLE('',#15996,12.499999999959);
#794=CIRCLE('',#15998,12.4999999999705);
#795=CIRCLE('',#15999,12.4999999999705);
#796=CIRCLE('',#16001,12.4999999999835);
#797=CIRCLE('',#16002,12.4999999999835);
#798=CIRCLE('',#16004,12.4999999999946);
#799=CIRCLE('',#16005,12.4999999999946);
#800=CIRCLE('',#16007,12.5000000000006);
#801=CIRCLE('',#16008,12.5000000000006);
#802=CIRCLE('',#16010,12.5);
#803=CIRCLE('',#16011,12.5);
#804=CIRCLE('',#16013,138.);
#805=CIRCLE('',#16014,138.);
#806=CIRCLE('',#16016,203.);
#807=CIRCLE('',#16017,203.);
#808=CIRCLE('',#16021,9.50000000000001);
#809=CIRCLE('',#16022,9.50000000000001);
#810=CIRCLE('',#16024,9.50000000000006);
#811=CIRCLE('',#16025,9.50000000000006);
#812=CIRCLE('',#16027,9.50000000000001);
#813=CIRCLE('',#16028,9.49999999999998);
#814=CIRCLE('',#16030,9.50000000000001);
#815=CIRCLE('',#16031,9.50000000000001);
#816=CIRCLE('',#16033,31.);
#817=CIRCLE('',#16034,31.);
#818=CIRCLE('',#16036,76.0000000000001);
#819=CIRCLE('',#16037,76.0000000000001);
#820=CIRCLE('',#16094,9.00000000000001);
#821=CIRCLE('',#16095,9.00000000000001);
#822=CIRCLE('',#16097,22.);
#823=CIRCLE('',#16098,22.);
#824=CIRCLE('',#16100,5.);
#825=CIRCLE('',#16101,5.);
#826=CIRCLE('',#16109,9.00000000000001);
#827=CIRCLE('',#16110,9.00000000000001);
#828=CIRCLE('',#16112,19.);
#829=CIRCLE('',#16114,19.);
#830=CIRCLE('',#16122,9.00000000000001);
#831=CIRCLE('',#16123,9.00000000000001);
#832=CIRCLE('',#16125,22.);
#833=CIRCLE('',#16126,22.);
#834=CIRCLE('',#16128,5.);
#835=CIRCLE('',#16129,5.);
#836=CIRCLE('',#16137,9.00000000000001);
#837=CIRCLE('',#16138,9.00000000000001);
#838=CIRCLE('',#16140,19.);
#839=CIRCLE('',#16142,19.);
#840=CIRCLE('',#16150,9.00000000000001);
#841=CIRCLE('',#16151,9.00000000000001);
#842=CIRCLE('',#16153,9.00000000000006);
#843=CIRCLE('',#16154,9.00000000000001);
#844=CIRCLE('',#16156,7.73750000000001);
#845=CIRCLE('',#16157,7.73750000000001);
#846=CIRCLE('',#16159,7.73750000000001);
#847=CIRCLE('',#16178,7.73750000000001);
#848=CIRCLE('',#16185,9.00000000000001);
#849=CIRCLE('',#16186,9.00000000000001);
#850=CIRCLE('',#16188,19.);
#851=CIRCLE('',#16190,19.);
#852=CIRCLE('',#16198,9.00000000000001);
#853=CIRCLE('',#16199,9.00000000000001);
#854=CIRCLE('',#16201,19.);
#855=CIRCLE('',#16203,19.);
#856=CIRCLE('',#16214,9.00000000000001);
#857=CIRCLE('',#16215,9.00000000000001);
#858=CIRCLE('',#16220,9.00000000000001);
#859=CIRCLE('',#16221,9.00000000000001);
#860=CIRCLE('',#16230,9.00000000000001);
#861=CIRCLE('',#16231,9.00000000000001);
#862=CIRCLE('',#16233,5.);
#863=CIRCLE('',#16234,5.);
#864=CIRCLE('',#16236,22.);
#865=CIRCLE('',#16237,22.);
#866=CIRCLE('',#16245,9.00000000000001);
#867=CIRCLE('',#16246,9.00000000000001);
#868=CIRCLE('',#16248,5.);
#869=CIRCLE('',#16249,5.);
#870=CIRCLE('',#16251,22.);
#871=CIRCLE('',#16252,22.);
#872=CIRCLE('',#16260,7.93749999999998);
#873=CIRCLE('',#16261,3.06250000000001);
#874=CIRCLE('',#16262,7.93749999999998);
#875=CIRCLE('',#16263,7.93749999999998);
#876=CIRCLE('',#16265,7.93749999999998);
#877=CIRCLE('',#16266,3.06250000000001);
#878=CIRCLE('',#16267,7.93749999999998);
#879=CIRCLE('',#16268,7.93749999999998);
#880=CIRCLE('',#16270,7.93749999999998);
#881=CIRCLE('',#16273,7.93749999999998);
#882=CIRCLE('',#16278,7.9375);
#883=CIRCLE('',#16279,7.09803);
#884=CIRCLE('',#16281,7.9375);
#885=CIRCLE('',#16291,13.4874);
#886=CIRCLE('',#16293,13.4874);
#887=CIRCLE('',#16295,13.4874);
#888=CIRCLE('',#16297,13.4874);
#889=CIRCLE('',#16299,13.4874);
#890=CIRCLE('',#16301,13.4874);
#891=CIRCLE('',#16305,7.9375);
#892=CIRCLE('',#16306,7.09803);
#893=CIRCLE('',#16308,7.9375);
#894=CIRCLE('',#16318,13.4874);
#895=CIRCLE('',#16320,13.4874);
#896=CIRCLE('',#16322,13.4874);
#897=CIRCLE('',#16324,13.4874);
#898=CIRCLE('',#16326,13.4874);
#899=CIRCLE('',#16328,13.4874);
#900=CIRCLE('',#16332,7.9375);
#901=CIRCLE('',#16333,7.9375);
#902=CIRCLE('',#16334,7.9375);
#903=CIRCLE('',#16336,7.34187);
#904=CIRCLE('',#16337,7.34187);
#905=CIRCLE('',#16339,7.34187);
#906=CIRCLE('',#16340,7.9375);
#907=CIRCLE('',#16349,11.9126);
#908=CIRCLE('',#16350,11.9126);
#909=CIRCLE('',#16351,11.9126);
#910=CIRCLE('',#16352,11.9126);
#911=CIRCLE('',#16353,11.9126);
#912=CIRCLE('',#16354,11.9126);
#913=CIRCLE('',#16356,11.9126);
#914=CIRCLE('',#16357,11.9126);
#915=CIRCLE('',#16358,11.9126);
#916=CIRCLE('',#16359,11.9126);
#917=CIRCLE('',#16360,11.9126);
#918=CIRCLE('',#16361,11.9126);
#919=CIRCLE('',#16376,6.56268467749802);
#920=CIRCLE('',#16419,7.9375);
#921=CIRCLE('',#16421,18.);
#922=CIRCLE('',#16422,3.);
#923=CIRCLE('',#16423,15.);
#924=CIRCLE('',#16424,3.);
#925=CIRCLE('',#16426,15.);
#926=CIRCLE('',#16427,3.);
#927=CIRCLE('',#16428,18.);
#928=CIRCLE('',#16429,3.);
#929=CIRCLE('',#16431,9.);
#930=CIRCLE('',#16432,9.);
#931=CIRCLE('',#16435,7.9375);
#932=CIRCLE('',#16436,4.93749999999999);
#933=CIRCLE('',#16443,1.5);
#934=CIRCLE('',#16444,1.5);
#935=CIRCLE('',#16445,1.5);
#936=CIRCLE('',#16446,1.5);
#937=CIRCLE('',#16447,3.);
#938=CIRCLE('',#16448,3.);
#939=CIRCLE('',#16449,3.);
#940=CIRCLE('',#16450,3.);
#941=CIRCLE('',#16453,6.56268467749995);
#942=CIRCLE('',#16458,6.56268467749995);
#943=CIRCLE('',#16460,7.9375);
#944=CIRCLE('',#16462,7.9375);
#945=CIRCLE('',#16467,7.9375);
#946=CIRCLE('',#16469,7.9375);
#947=CIRCLE('',#16470,4.93749999999997);
#948=CIRCLE('',#16472,7.9375);
#949=CIRCLE('',#16473,7.9375);
#950=CIRCLE('',#16475,4.93750000000002);
#951=CIRCLE('',#16478,4.93750000000002);
#952=CIRCLE('',#16481,12.246709909405);
#953=CIRCLE('',#16487,12.246709909405);
#954=CIRCLE('',#16488,12.246709909405);
#955=CIRCLE('',#16489,12.246709909405);
#956=CIRCLE('',#16490,12.246709909405);
#957=CIRCLE('',#16491,12.246709909405);
#958=CIRCLE('',#16492,12.246709909405);
#959=CIRCLE('',#16494,12.246709909405);
#960=CIRCLE('',#16495,12.246709909405);
#961=CIRCLE('',#16496,12.246709909405);
#962=CIRCLE('',#16497,12.246709909405);
#963=CIRCLE('',#16498,12.246709909405);
#964=CIRCLE('',#16499,12.246709909405);
#965=CIRCLE('',#16521,16.6624);
#966=CIRCLE('',#16522,16.6624);
#967=CIRCLE('',#16524,8.3312);
#968=CIRCLE('',#16525,8.3312);
#969=CIRCLE('',#16556,40.);
#970=CIRCLE('',#16557,40.);
#971=CIRCLE('',#16559,75.);
#972=CIRCLE('',#16561,75.);
#973=CIRCLE('',#16569,40.);
#974=CIRCLE('',#16570,40.);
#975=CIRCLE('',#16572,75.);
#976=CIRCLE('',#16574,75.);
#977=CIRCLE('',#16582,8.99999999999999);
#978=CIRCLE('',#16583,8.99999999999999);
#979=CIRCLE('',#16585,8.99999999999999);
#980=CIRCLE('',#16586,8.99999999999999);
#981=CIRCLE('',#16588,8.99999999999998);
#982=CIRCLE('',#16589,8.99999999999998);
#983=CIRCLE('',#16591,9.);
#984=CIRCLE('',#16592,8.99999999999999);
#985=CIRCLE('',#16594,8.99999999999999);
#986=CIRCLE('',#16595,8.99999999999999);
#987=CIRCLE('',#16627,8.99999999999997);
#988=CIRCLE('',#16628,8.99999999999997);
#989=CIRCLE('',#16630,8.99999999999999);
#990=CIRCLE('',#16631,8.99999999999999);
#991=CIRCLE('',#16633,8.99999999999997);
#992=CIRCLE('',#16634,8.99999999999997);
#993=CIRCLE('',#16642,8.99999999999998);
#994=CIRCLE('',#16643,8.99999999999998);
#995=CIRCLE('',#16645,9.);
#996=CIRCLE('',#16646,9.);
#997=CIRCLE('',#16648,8.99999999999995);
#998=CIRCLE('',#16649,8.99999999999995);
#999=CIRCLE('',#16657,8.99999999999998);
#1000=CIRCLE('',#16658,8.99999999999998);
#1001=CIRCLE('',#16660,8.99999999999999);
#1002=CIRCLE('',#16661,8.99999999999999);
#1003=CIRCLE('',#16663,8.99999999999997);
#1004=CIRCLE('',#16664,8.99999999999997);
#1005=CIRCLE('',#16672,8.99999999999998);
#1006=CIRCLE('',#16673,8.99999999999998);
#1007=CIRCLE('',#16675,9.);
#1008=CIRCLE('',#16676,9.);
#1009=CIRCLE('',#16678,8.99999999999995);
#1010=CIRCLE('',#16679,8.99999999999995);
#1011=CIRCLE('',#16717,9.00000000000004);
#1012=CIRCLE('',#16718,9.00000000000004);
#1013=CIRCLE('',#16720,9.00000000000004);
#1014=CIRCLE('',#16721,9.00000000000004);
#1015=CIRCLE('',#16723,9.00000000000006);
#1016=CIRCLE('',#16724,9.00000000000006);
#1017=CIRCLE('',#16726,9.00000000000006);
#1018=CIRCLE('',#16727,9.00000000000006);
#1019=CIRCLE('',#16735,9.00000000000004);
#1020=CIRCLE('',#16736,9.00000000000004);
#1021=CIRCLE('',#16738,9.00000000000004);
#1022=CIRCLE('',#16739,9.00000000000004);
#1023=CIRCLE('',#16741,9.00000000000004);
#1024=CIRCLE('',#16742,9.00000000000004);
#1025=CIRCLE('',#16744,9.00000000000004);
#1026=CIRCLE('',#16745,9.00000000000004);
#1027=CIRCLE('',#16747,9.00000000000004);
#1028=CIRCLE('',#16748,9.00000000000004);
#1029=CIRCLE('',#16750,9.00000000000004);
#1030=CIRCLE('',#16751,9.00000000000004);
#1031=CIRCLE('',#16858,9.00000000000004);
#1032=CIRCLE('',#16859,9.00000000000004);
#1033=CIRCLE('',#16861,9.00000000000004);
#1034=CIRCLE('',#16862,9.00000000000004);
#1035=CIRCLE('',#16864,9.00000000000006);
#1036=CIRCLE('',#16865,9.00000000000006);
#1037=CIRCLE('',#16867,9.00000000000006);
#1038=CIRCLE('',#16868,9.00000000000006);
#1039=CIRCLE('',#17009,8.);
#1040=CIRCLE('',#17010,8.);
#1041=CIRCLE('',#17011,1.2);
#1042=CIRCLE('',#17012,9.2);
#1043=CIRCLE('',#17014,13.5);
#1044=CIRCLE('',#17015,13.5);
#1045=CIRCLE('',#17016,13.5);
#1046=CIRCLE('',#17017,13.5);
#1047=CIRCLE('',#17018,13.5);
#1048=CIRCLE('',#17019,13.5);
#1049=CIRCLE('',#17020,13.5);
#1050=CIRCLE('',#17022,8.);
#1051=CIRCLE('',#17023,6.8985);
#1052=CIRCLE('',#17034,13.5);
#1053=CIRCLE('',#17035,13.5);
#1054=CIRCLE('',#17036,13.5);
#1055=CIRCLE('',#17037,13.5);
#1056=CIRCLE('',#17038,13.5);
#1057=CIRCLE('',#17039,13.5);
#1058=CIRCLE('',#17054,15.);
#1059=CIRCLE('',#17055,15.);
#1060=CIRCLE('',#17057,8.49999999999999);
#1061=CIRCLE('',#17058,8.49999999999999);
#1062=CIRCLE('',#17063,8.);
#1063=CIRCLE('',#17064,8.);
#1064=CIRCLE('',#17065,8.);
#1065=CIRCLE('',#17067,7.);
#1066=CIRCLE('',#17068,7.);
#1067=CIRCLE('',#17070,7.);
#1068=CIRCLE('',#17071,8.);
#1069=CIRCLE('',#17080,13.5);
#1070=CIRCLE('',#17081,13.5);
#1071=CIRCLE('',#17082,13.5);
#1072=CIRCLE('',#17083,13.5);
#1073=CIRCLE('',#17084,13.5);
#1074=CIRCLE('',#17085,13.5);
#1075=CIRCLE('',#17087,13.5);
#1076=CIRCLE('',#17088,13.5);
#1077=CIRCLE('',#17089,13.5);
#1078=CIRCLE('',#17090,13.5);
#1079=CIRCLE('',#17091,13.5);
#1080=CIRCLE('',#17092,13.5);
#1081=CYLINDRICAL_SURFACE('',#15797,75.0000000000001);
#1082=CYLINDRICAL_SURFACE('',#15807,75.0000000000001);
#1083=CYLINDRICAL_SURFACE('',#15815,8.99999999999998);
#1084=CYLINDRICAL_SURFACE('',#15818,8.99999999999998);
#1085=CYLINDRICAL_SURFACE('',#15821,8.99999999999998);
#1086=CYLINDRICAL_SURFACE('',#15824,8.99999999999998);
#1087=CYLINDRICAL_SURFACE('',#15827,8.99999999999998);
#1088=CYLINDRICAL_SURFACE('',#15830,8.99999999999998);
#1089=CYLINDRICAL_SURFACE('',#15839,8.99999999999998);
#1090=CYLINDRICAL_SURFACE('',#15842,9.00000000000001);
#1091=CYLINDRICAL_SURFACE('',#15845,9.00000000000001);
#1092=CYLINDRICAL_SURFACE('',#15848,9.00000000000001);
#1093=CYLINDRICAL_SURFACE('',#15851,9.00000000000001);
#1094=CYLINDRICAL_SURFACE('',#15860,8.99999999999998);
#1095=CYLINDRICAL_SURFACE('',#15863,9.00000000000001);
#1096=CYLINDRICAL_SURFACE('',#15866,9.00000000000001);
#1097=CYLINDRICAL_SURFACE('',#15869,9.00000000000001);
#1098=CYLINDRICAL_SURFACE('',#15872,9.00000000000001);
#1099=CYLINDRICAL_SURFACE('',#15900,9.00000000000006);
#1100=CYLINDRICAL_SURFACE('',#15903,9.00000000000006);
#1101=CYLINDRICAL_SURFACE('',#15906,9.00000000000005);
#1102=CYLINDRICAL_SURFACE('',#15909,9.00000000000005);
#1103=CYLINDRICAL_SURFACE('',#15912,9.00000000000006);
#1104=CYLINDRICAL_SURFACE('',#15915,9.00000000000006);
#1105=CYLINDRICAL_SURFACE('',#15918,9.00000000000006);
#1106=CYLINDRICAL_SURFACE('',#15921,9.00000000000006);
#1107=CYLINDRICAL_SURFACE('',#15924,9.00000000000006);
#1108=CYLINDRICAL_SURFACE('',#15927,9.00000000000006);
#1109=CYLINDRICAL_SURFACE('',#15930,9.00000000000406);
#1110=CYLINDRICAL_SURFACE('',#15933,9.00000000000006);
#1111=CYLINDRICAL_SURFACE('',#15936,9.00000000000006);
#1112=CYLINDRICAL_SURFACE('',#15939,9.00000000000006);
#1113=CYLINDRICAL_SURFACE('',#15942,9.00000000000006);
#1114=CYLINDRICAL_SURFACE('',#15945,31.0000000000001);
#1115=CYLINDRICAL_SURFACE('',#15948,138.);
#1116=CYLINDRICAL_SURFACE('',#15951,9.00000000000006);
#1117=CYLINDRICAL_SURFACE('',#15960,136.525);
#1118=CYLINDRICAL_SURFACE('',#15963,121.435);
#1119=CYLINDRICAL_SURFACE('',#15968,30.165);
#1120=CYLINDRICAL_SURFACE('',#15971,26.255);
#1121=CYLINDRICAL_SURFACE('',#15976,12.4999999999953);
#1122=CYLINDRICAL_SURFACE('',#15979,12.4999999999835);
#1123=CYLINDRICAL_SURFACE('',#15982,12.4999999999698);
#1124=CYLINDRICAL_SURFACE('',#15985,12.4999999999583);
#1125=CYLINDRICAL_SURFACE('',#15988,12.4999999999518);
#1126=CYLINDRICAL_SURFACE('',#15991,12.4999999999521);
#1127=CYLINDRICAL_SURFACE('',#15994,12.499999999959);
#1128=CYLINDRICAL_SURFACE('',#15997,12.4999999999705);
#1129=CYLINDRICAL_SURFACE('',#16000,12.4999999999835);
#1130=CYLINDRICAL_SURFACE('',#16003,12.4999999999946);
#1131=CYLINDRICAL_SURFACE('',#16006,12.5000000000006);
#1132=CYLINDRICAL_SURFACE('',#16009,12.5);
#1133=CYLINDRICAL_SURFACE('',#16012,138.);
#1134=CYLINDRICAL_SURFACE('',#16015,203.);
#1135=CYLINDRICAL_SURFACE('',#16020,9.50000000000001);
#1136=CYLINDRICAL_SURFACE('',#16023,9.50000000000006);
#1137=CYLINDRICAL_SURFACE('',#16026,9.50000000000001);
#1138=CYLINDRICAL_SURFACE('',#16029,9.50000000000001);
#1139=CYLINDRICAL_SURFACE('',#16032,31.);
#1140=CYLINDRICAL_SURFACE('',#16035,76.0000000000001);
#1141=CYLINDRICAL_SURFACE('',#16053,7.73749999999998);
#1142=CYLINDRICAL_SURFACE('',#16055,7.93749999999999);
#1143=CYLINDRICAL_SURFACE('',#16057,7.73750000000001);
#1144=CYLINDRICAL_SURFACE('',#16070,7.73749999999998);
#1145=CYLINDRICAL_SURFACE('',#16072,7.93750000000002);
#1146=CYLINDRICAL_SURFACE('',#16074,7.73750000000001);
#1147=CYLINDRICAL_SURFACE('',#16087,7.73749999999998);
#1148=CYLINDRICAL_SURFACE('',#16089,7.93750000000002);
#1149=CYLINDRICAL_SURFACE('',#16091,7.73750000000001);
#1150=CYLINDRICAL_SURFACE('',#16093,9.00000000000001);
#1151=CYLINDRICAL_SURFACE('',#16096,22.);
#1152=CYLINDRICAL_SURFACE('',#16099,5.);
#1153=CYLINDRICAL_SURFACE('',#16108,9.00000000000001);
#1154=CYLINDRICAL_SURFACE('',#16118,19.);
#1155=CYLINDRICAL_SURFACE('',#16121,9.00000000000001);
#1156=CYLINDRICAL_SURFACE('',#16124,22.);
#1157=CYLINDRICAL_SURFACE('',#16127,5.);
#1158=CYLINDRICAL_SURFACE('',#16136,9.00000000000001);
#1159=CYLINDRICAL_SURFACE('',#16146,19.);
#1160=CYLINDRICAL_SURFACE('',#16149,9.00000000000001);
#1161=CYLINDRICAL_SURFACE('',#16152,9.00000000000006);
#1162=CYLINDRICAL_SURFACE('',#16155,7.73750000000001);
#1163=CYLINDRICAL_SURFACE('',#16158,7.73750000000001);
#1164=CYLINDRICAL_SURFACE('',#16173,7.73749999999998);
#1165=CYLINDRICAL_SURFACE('',#16175,7.93749999999999);
#1166=CYLINDRICAL_SURFACE('',#16177,7.73750000000001);
#1167=CYLINDRICAL_SURFACE('',#16184,9.00000000000001);
#1168=CYLINDRICAL_SURFACE('',#16194,19.);
#1169=CYLINDRICAL_SURFACE('',#16197,9.00000000000001);
#1170=CYLINDRICAL_SURFACE('',#16207,19.);
#1171=CYLINDRICAL_SURFACE('',#16213,9.00000000000001);
#1172=CYLINDRICAL_SURFACE('',#16219,9.00000000000001);
#1173=CYLINDRICAL_SURFACE('',#16229,9.00000000000001);
#1174=CYLINDRICAL_SURFACE('',#16232,5.);
#1175=CYLINDRICAL_SURFACE('',#16235,22.);
#1176=CYLINDRICAL_SURFACE('',#16244,9.00000000000001);
#1177=CYLINDRICAL_SURFACE('',#16247,5.);
#1178=CYLINDRICAL_SURFACE('',#16250,22.);
#1179=CYLINDRICAL_SURFACE('',#16269,7.93749999999998);
#1180=CYLINDRICAL_SURFACE('',#16271,7.93749999999999);
#1181=CYLINDRICAL_SURFACE('',#16272,7.93749999999998);
#1182=CYLINDRICAL_SURFACE('',#16280,7.9375);
#1183=CYLINDRICAL_SURFACE('',#16307,7.9375);
#1184=CYLINDRICAL_SURFACE('',#16331,7.9375);
#1185=CYLINDRICAL_SURFACE('',#16341,7.34187);
#1186=CYLINDRICAL_SURFACE('',#16375,6.56268467496113);
#1187=CYLINDRICAL_SURFACE('',#16377,6.56268467496113);
#1188=CYLINDRICAL_SURFACE('',#16378,6.56268467496113);
#1189=CYLINDRICAL_SURFACE('',#16379,6.56268467496113);
#1190=CYLINDRICAL_SURFACE('',#16380,6.56268467496113);
#1191=CYLINDRICAL_SURFACE('',#16381,6.56268467496113);
#1192=CYLINDRICAL_SURFACE('',#16382,6.56268467496113);
#1193=CYLINDRICAL_SURFACE('',#16383,6.56268467496113);
#1194=CYLINDRICAL_SURFACE('',#16384,6.56268467496113);
#1195=CYLINDRICAL_SURFACE('',#16385,6.56268467496113);
#1196=CYLINDRICAL_SURFACE('',#16386,6.56268467496113);
#1197=CYLINDRICAL_SURFACE('',#16387,6.56268467496113);
#1198=CYLINDRICAL_SURFACE('',#16388,6.56268467496113);
#1199=CYLINDRICAL_SURFACE('',#16389,6.56268467496113);
#1200=CYLINDRICAL_SURFACE('',#16390,6.56268467496113);
#1201=CYLINDRICAL_SURFACE('',#16391,6.56268467496113);
#1202=CYLINDRICAL_SURFACE('',#16392,6.56268467496113);
#1203=CYLINDRICAL_SURFACE('',#16393,6.56268467496113);
#1204=CYLINDRICAL_SURFACE('',#16394,6.56268467496113);
#1205=CYLINDRICAL_SURFACE('',#16395,6.56268467496113);
#1206=CYLINDRICAL_SURFACE('',#16396,6.56268467496113);
#1207=CYLINDRICAL_SURFACE('',#16397,6.56268467496113);
#1208=CYLINDRICAL_SURFACE('',#16398,7.9375);
#1209=CYLINDRICAL_SURFACE('',#16399,7.9375);
#1210=CYLINDRICAL_SURFACE('',#16400,7.9375);
#1211=CYLINDRICAL_SURFACE('',#16401,7.9375);
#1212=CYLINDRICAL_SURFACE('',#16402,7.9375);
#1213=CYLINDRICAL_SURFACE('',#16403,7.9375);
#1214=CYLINDRICAL_SURFACE('',#16404,7.9375);
#1215=CYLINDRICAL_SURFACE('',#16405,7.9375);
#1216=CYLINDRICAL_SURFACE('',#16406,7.9375);
#1217=CYLINDRICAL_SURFACE('',#16407,7.9375);
#1218=CYLINDRICAL_SURFACE('',#16408,7.9375);
#1219=CYLINDRICAL_SURFACE('',#16409,7.9375);
#1220=CYLINDRICAL_SURFACE('',#16410,7.9375);
#1221=CYLINDRICAL_SURFACE('',#16411,7.9375);
#1222=CYLINDRICAL_SURFACE('',#16412,7.9375);
#1223=CYLINDRICAL_SURFACE('',#16413,7.9375);
#1224=CYLINDRICAL_SURFACE('',#16414,7.9375);
#1225=CYLINDRICAL_SURFACE('',#16415,7.9375);
#1226=CYLINDRICAL_SURFACE('',#16416,7.9375);
#1227=CYLINDRICAL_SURFACE('',#16417,7.9375);
#1228=CYLINDRICAL_SURFACE('',#16418,7.9375);
#1229=CYLINDRICAL_SURFACE('',#16430,9.);
#1230=CYLINDRICAL_SURFACE('',#16433,18.);
#1231=CYLINDRICAL_SURFACE('',#16437,7.9375);
#1232=CYLINDRICAL_SURFACE('',#16442,6.56268467496113);
#1233=CYLINDRICAL_SURFACE('',#16452,6.56268467749995);
#1234=CYLINDRICAL_SURFACE('',#16454,6.56268467749995);
#1235=CYLINDRICAL_SURFACE('',#16455,6.56268467749995);
#1236=CYLINDRICAL_SURFACE('',#16456,6.56268467749995);
#1237=CYLINDRICAL_SURFACE('',#16457,6.56268467749995);
#1238=CYLINDRICAL_SURFACE('',#16459,7.9375);
#1239=CYLINDRICAL_SURFACE('',#16461,7.9375);
#1240=CYLINDRICAL_SURFACE('',#16463,7.9375);
#1241=CYLINDRICAL_SURFACE('',#16464,7.9375);
#1242=CYLINDRICAL_SURFACE('',#16465,7.9375);
#1243=CYLINDRICAL_SURFACE('',#16466,7.9375);
#1244=CYLINDRICAL_SURFACE('',#16471,7.9375);
#1245=CYLINDRICAL_SURFACE('',#16479,7.9375);
#1246=CYLINDRICAL_SURFACE('',#16516,6.56268467749995);
#1247=CYLINDRICAL_SURFACE('',#16517,4.93750000000002);
#1248=CYLINDRICAL_SURFACE('',#16520,16.6624);
#1249=CYLINDRICAL_SURFACE('',#16523,8.3312);
#1250=CYLINDRICAL_SURFACE('',#16555,40.);
#1251=CYLINDRICAL_SURFACE('',#16566,75.);
#1252=CYLINDRICAL_SURFACE('',#16568,40.);
#1253=CYLINDRICAL_SURFACE('',#16579,75.);
#1254=CYLINDRICAL_SURFACE('',#16581,8.99999999999999);
#1255=CYLINDRICAL_SURFACE('',#16584,8.99999999999999);
#1256=CYLINDRICAL_SURFACE('',#16587,8.99999999999998);
#1257=CYLINDRICAL_SURFACE('',#16590,9.);
#1258=CYLINDRICAL_SURFACE('',#16593,8.99999999999999);
#1259=CYLINDRICAL_SURFACE('',#16626,8.99999999999997);
#1260=CYLINDRICAL_SURFACE('',#16629,8.99999999999999);
#1261=CYLINDRICAL_SURFACE('',#16632,8.99999999999997);
#1262=CYLINDRICAL_SURFACE('',#16641,8.99999999999998);
#1263=CYLINDRICAL_SURFACE('',#16644,9.);
#1264=CYLINDRICAL_SURFACE('',#16647,8.99999999999995);
#1265=CYLINDRICAL_SURFACE('',#16656,8.99999999999998);
#1266=CYLINDRICAL_SURFACE('',#16659,8.99999999999999);
#1267=CYLINDRICAL_SURFACE('',#16662,8.99999999999997);
#1268=CYLINDRICAL_SURFACE('',#16671,8.99999999999998);
#1269=CYLINDRICAL_SURFACE('',#16674,9.);
#1270=CYLINDRICAL_SURFACE('',#16677,8.99999999999996);
#1271=CYLINDRICAL_SURFACE('',#16716,9.00000000000004);
#1272=CYLINDRICAL_SURFACE('',#16719,9.00000000000004);
#1273=CYLINDRICAL_SURFACE('',#16722,9.00000000000006);
#1274=CYLINDRICAL_SURFACE('',#16725,9.00000000000006);
#1275=CYLINDRICAL_SURFACE('',#16734,9.00000000000004);
#1276=CYLINDRICAL_SURFACE('',#16737,9.00000000000004);
#1277=CYLINDRICAL_SURFACE('',#16740,9.00000000000004);
#1278=CYLINDRICAL_SURFACE('',#16743,9.00000000000004);
#1279=CYLINDRICAL_SURFACE('',#16746,9.00000000000004);
#1280=CYLINDRICAL_SURFACE('',#16749,9.00000000000004);
#1281=CYLINDRICAL_SURFACE('',#16857,9.00000000000004);
#1282=CYLINDRICAL_SURFACE('',#16860,9.00000000000004);
#1283=CYLINDRICAL_SURFACE('',#16863,9.00000000000006);
#1284=CYLINDRICAL_SURFACE('',#16866,9.00000000000006);
#1285=CYLINDRICAL_SURFACE('',#17013,13.5);
#1286=CYLINDRICAL_SURFACE('',#17024,8.);
#1287=CYLINDRICAL_SURFACE('',#17053,15.);
#1288=CYLINDRICAL_SURFACE('',#17056,8.49999999999999);
#1289=CYLINDRICAL_SURFACE('',#17062,8.);
#1290=CYLINDRICAL_SURFACE('',#17072,7.);
#1291=STYLED_ITEM('',(#33097),#1380);
#1292=STYLED_ITEM('',(#33097),#1381);
#1293=STYLED_ITEM('',(#33097),#1382);
#1294=STYLED_ITEM('',(#33097),#1383);
#1295=STYLED_ITEM('',(#33097),#1384);
#1296=STYLED_ITEM('',(#33097),#1385);
#1297=STYLED_ITEM('',(#33097),#1386);
#1298=STYLED_ITEM('',(#33097),#1387);
#1299=STYLED_ITEM('',(#33097),#1388);
#1300=STYLED_ITEM('',(#33097),#1389);
#1301=STYLED_ITEM('',(#33097),#1390);
#1302=STYLED_ITEM('',(#33097),#1391);
#1303=STYLED_ITEM('',(#33097),#1392);
#1304=STYLED_ITEM('',(#33097),#1393);
#1305=STYLED_ITEM('',(#33098),#1394);
#1306=STYLED_ITEM('',(#33098),#1395);
#1307=STYLED_ITEM('',(#33098),#1396);
#1308=STYLED_ITEM('',(#33098),#1397);
#1309=STYLED_ITEM('',(#33098),#1398);
#1310=STYLED_ITEM('',(#33098),#1399);
#1311=STYLED_ITEM('',(#33098),#1400);
#1312=STYLED_ITEM('',(#33098),#1401);
#1313=STYLED_ITEM('',(#33098),#1402);
#1314=STYLED_ITEM('',(#33098),#1403);
#1315=STYLED_ITEM('',(#33098),#1404);
#1316=STYLED_ITEM('',(#33098),#1405);
#1317=STYLED_ITEM('',(#33098),#1406);
#1318=STYLED_ITEM('',(#33098),#1407);
#1319=STYLED_ITEM('',(#33099),#1408);
#1320=STYLED_ITEM('',(#33099),#1409);
#1321=STYLED_ITEM('',(#33099),#1410);
#1322=STYLED_ITEM('',(#33098),#1411);
#1323=STYLED_ITEM('',(#33100),#1412);
#1324=STYLED_ITEM('',(#33099),#1413);
#1325=STYLED_ITEM('',(#33101),#1414);
#1326=STYLED_ITEM('',(#33101),#1415);
#1327=STYLED_ITEM('',(#33101),#1416);
#1328=STYLED_ITEM('',(#33101),#1417);
#1329=STYLED_ITEM('',(#33101),#1418);
#1330=STYLED_ITEM('',(#33101),#1419);
#1331=STYLED_ITEM('',(#33101),#1420);
#1332=STYLED_ITEM('',(#33101),#1421);
#1333=STYLED_ITEM('',(#33101),#1422);
#1334=STYLED_ITEM('',(#33101),#1423);
#1335=STYLED_ITEM('',(#33101),#1424);
#1336=STYLED_ITEM('',(#33101),#1425);
#1337=STYLED_ITEM('',(#33101),#1426);
#1338=STYLED_ITEM('',(#33101),#1427);
#1339=STYLED_ITEM('',(#33101),#1428);
#1340=STYLED_ITEM('',(#33101),#1429);
#1341=STYLED_ITEM('',(#33101),#1430);
#1342=STYLED_ITEM('',(#33101),#1431);
#1343=STYLED_ITEM('',(#33101),#1432);
#1344=STYLED_ITEM('',(#33101),#1433);
#1345=STYLED_ITEM('',(#33101),#1434);
#1346=STYLED_ITEM('',(#33101),#1435);
#1347=STYLED_ITEM('',(#33101),#1436);
#1348=STYLED_ITEM('',(#33101),#1437);
#1349=STYLED_ITEM('',(#33101),#1438);
#1350=STYLED_ITEM('',(#33101),#1439);
#1351=STYLED_ITEM('',(#33101),#1440);
#1352=STYLED_ITEM('',(#33101),#1441);
#1353=STYLED_ITEM('',(#33101),#1442);
#1354=STYLED_ITEM('',(#33101),#1443);
#1355=STYLED_ITEM('',(#33101),#1444);
#1356=STYLED_ITEM('',(#33101),#1445);
#1357=STYLED_ITEM('',(#33101),#1446);
#1358=STYLED_ITEM('',(#33101),#1447);
#1359=STYLED_ITEM('',(#33101),#1448);
#1360=STYLED_ITEM('',(#33101),#1449);
#1361=STYLED_ITEM('',(#33101),#1450);
#1362=STYLED_ITEM('',(#33101),#1451);
#1363=STYLED_ITEM('',(#33101),#1452);
#1364=STYLED_ITEM('',(#33101),#1453);
#1365=STYLED_ITEM('',(#33101),#1454);
#1366=STYLED_ITEM('',(#33101),#1455);
#1367=STYLED_ITEM('',(#33101),#1456);
#1368=STYLED_ITEM('',(#33101),#1457);
#1369=STYLED_ITEM('',(#33101),#1458);
#1370=STYLED_ITEM('',(#33101),#1459);
#1371=STYLED_ITEM('',(#33101),#1460);
#1372=STYLED_ITEM('',(#33101),#1461);
#1373=STYLED_ITEM('',(#33101),#1462);
#1374=STYLED_ITEM('',(#33101),#1463);
#1375=STYLED_ITEM('',(#33101),#1464);
#1376=STYLED_ITEM('',(#33101),#1465);
#1377=STYLED_ITEM('',(#33099),#1466);
#1378=STYLED_ITEM('',(#33099),#1467);
#1379=STYLED_ITEM('',(#33099),#1468);
#1380=MANIFOLD_SOLID_BREP('Body1',#15539);
#1381=MANIFOLD_SOLID_BREP('Body2',#15540);
#1382=MANIFOLD_SOLID_BREP('Body3',#15541);
#1383=MANIFOLD_SOLID_BREP('Body4',#15542);
#1384=MANIFOLD_SOLID_BREP('Body5',#15543);
#1385=MANIFOLD_SOLID_BREP('Body6',#15544);
#1386=MANIFOLD_SOLID_BREP('Body7',#15545);
#1387=MANIFOLD_SOLID_BREP('Body8',#15546);
#1388=MANIFOLD_SOLID_BREP('Body9',#15547);
#1389=MANIFOLD_SOLID_BREP('Body1',#15548);
#1390=MANIFOLD_SOLID_BREP('Body2',#15549);
#1391=MANIFOLD_SOLID_BREP('Body3',#15550);
#1392=MANIFOLD_SOLID_BREP('Body4',#15551);
#1393=MANIFOLD_SOLID_BREP('Body5',#15552);
#1394=MANIFOLD_SOLID_BREP('Body1',#15553);
#1395=MANIFOLD_SOLID_BREP('Body2',#15554);
#1396=MANIFOLD_SOLID_BREP('Body3',#15555);
#1397=MANIFOLD_SOLID_BREP('Body4',#15556);
#1398=MANIFOLD_SOLID_BREP('Body5',#15557);
#1399=MANIFOLD_SOLID_BREP('Body6',#15558);
#1400=MANIFOLD_SOLID_BREP('Body7',#15559);
#1401=MANIFOLD_SOLID_BREP('Body8',#15560);
#1402=MANIFOLD_SOLID_BREP('Body9',#15561);
#1403=MANIFOLD_SOLID_BREP('Body10',#15562);
#1404=MANIFOLD_SOLID_BREP('Body1',#15563);
#1405=MANIFOLD_SOLID_BREP('Body2',#15564);
#1406=MANIFOLD_SOLID_BREP('Body3',#15565);
#1407=MANIFOLD_SOLID_BREP('Body4',#15566);
#1408=MANIFOLD_SOLID_BREP('Body1',#15567);
#1409=MANIFOLD_SOLID_BREP('Body1',#15568);
#1410=MANIFOLD_SOLID_BREP('Body1',#15569);
#1411=MANIFOLD_SOLID_BREP('Body1',#15570);
#1412=MANIFOLD_SOLID_BREP('Body1',#15571);
#1413=MANIFOLD_SOLID_BREP('Body1',#15572);
#1414=MANIFOLD_SOLID_BREP('Body1',#15573);
#1415=MANIFOLD_SOLID_BREP('Body2',#15574);
#1416=MANIFOLD_SOLID_BREP('Body3',#15575);
#1417=MANIFOLD_SOLID_BREP('Body4',#15576);
#1418=MANIFOLD_SOLID_BREP('Body5',#15577);
#1419=MANIFOLD_SOLID_BREP('Body6',#15578);
#1420=MANIFOLD_SOLID_BREP('Body7',#15579);
#1421=MANIFOLD_SOLID_BREP('Body8',#15580);
#1422=MANIFOLD_SOLID_BREP('Body9',#15581);
#1423=MANIFOLD_SOLID_BREP('Body10',#15582);
#1424=MANIFOLD_SOLID_BREP('Body11',#15583);
#1425=MANIFOLD_SOLID_BREP('Body12',#15584);
#1426=MANIFOLD_SOLID_BREP('Body13',#15585);
#1427=MANIFOLD_SOLID_BREP('Body14',#15586);
#1428=MANIFOLD_SOLID_BREP('Body15',#15587);
#1429=MANIFOLD_SOLID_BREP('Body16',#15588);
#1430=MANIFOLD_SOLID_BREP('Body17',#15589);
#1431=MANIFOLD_SOLID_BREP('Body18',#15590);
#1432=MANIFOLD_SOLID_BREP('Body19',#15591);
#1433=MANIFOLD_SOLID_BREP('Body20',#15592);
#1434=MANIFOLD_SOLID_BREP('Body21',#15593);
#1435=MANIFOLD_SOLID_BREP('Body22',#15594);
#1436=MANIFOLD_SOLID_BREP('Body23',#15595);
#1437=MANIFOLD_SOLID_BREP('Body24',#15596);
#1438=MANIFOLD_SOLID_BREP('Body25',#15597);
#1439=MANIFOLD_SOLID_BREP('Body26',#15598);
#1440=MANIFOLD_SOLID_BREP('Body27',#15599);
#1441=MANIFOLD_SOLID_BREP('Body28',#15600);
#1442=MANIFOLD_SOLID_BREP('Body29',#15601);
#1443=MANIFOLD_SOLID_BREP('Body30',#15602);
#1444=MANIFOLD_SOLID_BREP('Body31',#15603);
#1445=MANIFOLD_SOLID_BREP('Body32',#15604);
#1446=MANIFOLD_SOLID_BREP('Body33',#15605);
#1447=MANIFOLD_SOLID_BREP('Body34',#15606);
#1448=MANIFOLD_SOLID_BREP('Body35',#15607);
#1449=MANIFOLD_SOLID_BREP('Body36',#15608);
#1450=MANIFOLD_SOLID_BREP('Body37',#15609);
#1451=MANIFOLD_SOLID_BREP('Body38',#15610);
#1452=MANIFOLD_SOLID_BREP('Body39',#15611);
#1453=MANIFOLD_SOLID_BREP('Body40',#15612);
#1454=MANIFOLD_SOLID_BREP('Body41',#15613);
#1455=MANIFOLD_SOLID_BREP('Body42',#15614);
#1456=MANIFOLD_SOLID_BREP('Body43',#15615);
#1457=MANIFOLD_SOLID_BREP('Body44',#15616);
#1458=MANIFOLD_SOLID_BREP('Body45',#15617);
#1459=MANIFOLD_SOLID_BREP('Body46',#15618);
#1460=MANIFOLD_SOLID_BREP('Body47',#15619);
#1461=MANIFOLD_SOLID_BREP('Body48',#15620);
#1462=MANIFOLD_SOLID_BREP('Body49',#15621);
#1463=MANIFOLD_SOLID_BREP('Body50',#15622);
#1464=MANIFOLD_SOLID_BREP('Body51',#15623);
#1465=MANIFOLD_SOLID_BREP('Body52',#15624);
#1466=MANIFOLD_SOLID_BREP('Body1',#15625);
#1467=MANIFOLD_SOLID_BREP('Body1',#15626);
#1468=MANIFOLD_SOLID_BREP('Body1',#15627);
#1469=FACE_BOUND('',#2576,.T.);
#1470=FACE_BOUND('',#2578,.T.);
#1471=FACE_BOUND('',#2606,.T.);
#1472=FACE_BOUND('',#2607,.T.);
#1473=FACE_BOUND('',#2608,.T.);
#1474=FACE_BOUND('',#2609,.T.);
#1475=FACE_BOUND('',#2610,.T.);
#1476=FACE_BOUND('',#2611,.T.);
#1477=FACE_BOUND('',#2613,.T.);
#1478=FACE_BOUND('',#2614,.T.);
#1479=FACE_BOUND('',#2615,.T.);
#1480=FACE_BOUND('',#2616,.T.);
#1481=FACE_BOUND('',#2617,.T.);
#1482=FACE_BOUND('',#2618,.T.);
#1483=FACE_BOUND('',#2633,.T.);
#1484=FACE_BOUND('',#2634,.T.);
#1485=FACE_BOUND('',#2635,.T.);
#1486=FACE_BOUND('',#2636,.T.);
#1487=FACE_BOUND('',#2637,.T.);
#1488=FACE_BOUND('',#2639,.T.);
#1489=FACE_BOUND('',#2640,.T.);
#1490=FACE_BOUND('',#2641,.T.);
#1491=FACE_BOUND('',#2642,.T.);
#1492=FACE_BOUND('',#2643,.T.);
#1493=FACE_BOUND('',#2654,.T.);
#1494=FACE_BOUND('',#2655,.T.);
#1495=FACE_BOUND('',#2656,.T.);
#1496=FACE_BOUND('',#2657,.T.);
#1497=FACE_BOUND('',#2658,.T.);
#1498=FACE_BOUND('',#2660,.T.);
#1499=FACE_BOUND('',#2661,.T.);
#1500=FACE_BOUND('',#2662,.T.);
#1501=FACE_BOUND('',#2663,.T.);
#1502=FACE_BOUND('',#2664,.T.);
#1503=FACE_BOUND('',#2706,.T.);
#1504=FACE_BOUND('',#2707,.T.);
#1505=FACE_BOUND('',#2708,.T.);
#1506=FACE_BOUND('',#2709,.T.);
#1507=FACE_BOUND('',#2710,.T.);
#1508=FACE_BOUND('',#2711,.T.);
#1509=FACE_BOUND('',#2712,.T.);
#1510=FACE_BOUND('',#2713,.T.);
#1511=FACE_BOUND('',#2714,.T.);
#1512=FACE_BOUND('',#2715,.T.);
#1513=FACE_BOUND('',#2716,.T.);
#1514=FACE_BOUND('',#2717,.T.);
#1515=FACE_BOUND('',#2718,.T.);
#1516=FACE_BOUND('',#2719,.T.);
#1517=FACE_BOUND('',#2720,.T.);
#1518=FACE_BOUND('',#2721,.T.);
#1519=FACE_BOUND('',#2722,.T.);
#1520=FACE_BOUND('',#2723,.T.);
#1521=FACE_BOUND('',#2725,.T.);
#1522=FACE_BOUND('',#2726,.T.);
#1523=FACE_BOUND('',#2727,.T.);
#1524=FACE_BOUND('',#2728,.T.);
#1525=FACE_BOUND('',#2729,.T.);
#1526=FACE_BOUND('',#2730,.T.);
#1527=FACE_BOUND('',#2731,.T.);
#1528=FACE_BOUND('',#2732,.T.);
#1529=FACE_BOUND('',#2733,.T.);
#1530=FACE_BOUND('',#2734,.T.);
#1531=FACE_BOUND('',#2735,.T.);
#1532=FACE_BOUND('',#2736,.T.);
#1533=FACE_BOUND('',#2737,.T.);
#1534=FACE_BOUND('',#2738,.T.);
#1535=FACE_BOUND('',#2739,.T.);
#1536=FACE_BOUND('',#2740,.T.);
#1537=FACE_BOUND('',#2741,.T.);
#1538=FACE_BOUND('',#2742,.T.);
#1539=FACE_BOUND('',#2746,.T.);
#1540=FACE_BOUND('',#2748,.T.);
#1541=FACE_BOUND('',#2752,.T.);
#1542=FACE_BOUND('',#2754,.T.);
#1543=FACE_BOUND('',#2770,.T.);
#1544=FACE_BOUND('',#2771,.T.);
#1545=FACE_BOUND('',#2772,.T.);
#1546=FACE_BOUND('',#2773,.T.);
#1547=FACE_BOUND('',#2774,.T.);
#1548=FACE_BOUND('',#2775,.T.);
#1549=FACE_BOUND('',#2776,.T.);
#1550=FACE_BOUND('',#2777,.T.);
#1551=FACE_BOUND('',#2778,.T.);
#1552=FACE_BOUND('',#2779,.T.);
#1553=FACE_BOUND('',#2780,.T.);
#1554=FACE_BOUND('',#2781,.T.);
#1555=FACE_BOUND('',#2782,.T.);
#1556=FACE_BOUND('',#2784,.T.);
#1557=FACE_BOUND('',#2785,.T.);
#1558=FACE_BOUND('',#2786,.T.);
#1559=FACE_BOUND('',#2787,.T.);
#1560=FACE_BOUND('',#2788,.T.);
#1561=FACE_BOUND('',#2789,.T.);
#1562=FACE_BOUND('',#2790,.T.);
#1563=FACE_BOUND('',#2791,.T.);
#1564=FACE_BOUND('',#2792,.T.);
#1565=FACE_BOUND('',#2793,.T.);
#1566=FACE_BOUND('',#2794,.T.);
#1567=FACE_BOUND('',#2795,.T.);
#1568=FACE_BOUND('',#2796,.T.);
#1569=FACE_BOUND('',#2804,.T.);
#1570=FACE_BOUND('',#2805,.T.);
#1571=FACE_BOUND('',#2806,.T.);
#1572=FACE_BOUND('',#2807,.T.);
#1573=FACE_BOUND('',#2808,.T.);
#1574=FACE_BOUND('',#2810,.T.);
#1575=FACE_BOUND('',#2811,.T.);
#1576=FACE_BOUND('',#2812,.T.);
#1577=FACE_BOUND('',#2813,.T.);
#1578=FACE_BOUND('',#2814,.T.);
#1579=FACE_BOUND('',#2856,.T.);
#1580=FACE_BOUND('',#2858,.T.);
#1581=FACE_BOUND('',#2861,.T.);
#1582=FACE_BOUND('',#2863,.T.);
#1583=FACE_BOUND('',#2878,.T.);
#1584=FACE_BOUND('',#2880,.T.);
#1585=FACE_BOUND('',#2883,.T.);
#1586=FACE_BOUND('',#2885,.T.);
#1587=FACE_BOUND('',#2915,.T.);
#1588=FACE_BOUND('',#2917,.T.);
#1589=FACE_BOUND('',#2926,.T.);
#1590=FACE_BOUND('',#2928,.T.);
#1591=FACE_BOUND('',#2953,.T.);
#1592=FACE_BOUND('',#2955,.T.);
#1593=FACE_BOUND('',#2964,.T.);
#1594=FACE_BOUND('',#2966,.T.);
#1595=FACE_BOUND('',#2987,.T.);
#1596=FACE_BOUND('',#3005,.T.);
#1597=FACE_BOUND('',#3025,.T.);
#1598=FACE_BOUND('',#3027,.T.);
#1599=FACE_BOUND('',#3090,.T.);
#1600=FACE_BOUND('',#3092,.T.);
#1601=FACE_BOUND('',#3131,.T.);
#1602=FACE_BOUND('',#3133,.T.);
#1603=FACE_BOUND('',#3158,.T.);
#1604=FACE_BOUND('',#3160,.T.);
#1605=FACE_BOUND('',#3169,.T.);
#1606=FACE_BOUND('',#3171,.T.);
#1607=FACE_BOUND('',#3180,.T.);
#1608=FACE_BOUND('',#3182,.T.);
#1609=FACE_BOUND('',#3195,.T.);
#1610=FACE_BOUND('',#3196,.T.);
#1611=FACE_BOUND('',#3197,.T.);
#1612=FACE_BOUND('',#3198,.T.);
#1613=FACE_BOUND('',#3199,.T.);
#1614=FACE_BOUND('',#3201,.T.);
#1615=FACE_BOUND('',#3202,.T.);
#1616=FACE_BOUND('',#3203,.T.);
#1617=FACE_BOUND('',#3204,.T.);
#1618=FACE_BOUND('',#3205,.T.);
#1619=FACE_BOUND('',#3238,.T.);
#1620=FACE_BOUND('',#3239,.T.);
#1621=FACE_BOUND('',#3240,.T.);
#1622=FACE_BOUND('',#3242,.T.);
#1623=FACE_BOUND('',#3243,.T.);
#1624=FACE_BOUND('',#3244,.T.);
#1625=FACE_BOUND('',#3253,.T.);
#1626=FACE_BOUND('',#3254,.T.);
#1627=FACE_BOUND('',#3255,.T.);
#1628=FACE_BOUND('',#3257,.T.);
#1629=FACE_BOUND('',#3258,.T.);
#1630=FACE_BOUND('',#3259,.T.);
#1631=FACE_BOUND('',#3268,.T.);
#1632=FACE_BOUND('',#3269,.T.);
#1633=FACE_BOUND('',#3270,.T.);
#1634=FACE_BOUND('',#3272,.T.);
#1635=FACE_BOUND('',#3273,.T.);
#1636=FACE_BOUND('',#3274,.T.);
#1637=FACE_BOUND('',#3283,.T.);
#1638=FACE_BOUND('',#3284,.T.);
#1639=FACE_BOUND('',#3285,.T.);
#1640=FACE_BOUND('',#3287,.T.);
#1641=FACE_BOUND('',#3288,.T.);
#1642=FACE_BOUND('',#3289,.T.);
#1643=FACE_BOUND('',#3329,.T.);
#1644=FACE_BOUND('',#3330,.T.);
#1645=FACE_BOUND('',#3331,.T.);
#1646=FACE_BOUND('',#3332,.T.);
#1647=FACE_BOUND('',#3334,.T.);
#1648=FACE_BOUND('',#3335,.T.);
#1649=FACE_BOUND('',#3336,.T.);
#1650=FACE_BOUND('',#3337,.T.);
#1651=FACE_BOUND('',#3353,.T.);
#1652=FACE_BOUND('',#3354,.T.);
#1653=FACE_BOUND('',#3355,.T.);
#1654=FACE_BOUND('',#3356,.T.);
#1655=FACE_BOUND('',#3357,.T.);
#1656=FACE_BOUND('',#3358,.T.);
#1657=FACE_BOUND('',#3360,.T.);
#1658=FACE_BOUND('',#3361,.T.);
#1659=FACE_BOUND('',#3362,.T.);
#1660=FACE_BOUND('',#3363,.T.);
#1661=FACE_BOUND('',#3364,.T.);
#1662=FACE_BOUND('',#3365,.T.);
#1663=FACE_BOUND('',#3470,.T.);
#1664=FACE_BOUND('',#3471,.T.);
#1665=FACE_BOUND('',#3472,.T.);
#1666=FACE_BOUND('',#3473,.T.);
#1667=FACE_BOUND('',#3475,.T.);
#1668=FACE_BOUND('',#3476,.T.);
#1669=FACE_BOUND('',#3477,.T.);
#1670=FACE_BOUND('',#3478,.T.);
#1671=FACE_BOUND('',#3620,.T.);
#1672=FACE_BOUND('',#3644,.T.);
#1673=FACE_BOUND('',#3646,.T.);
#1674=FACE_BOUND('',#3658,.T.);
#1675=FACE_BOUND('',#3660,.T.);
#1676=FACE_OUTER_BOUND('',#2571,.T.);
#1677=FACE_OUTER_BOUND('',#2572,.T.);
#1678=FACE_OUTER_BOUND('',#2573,.T.);
#1679=FACE_OUTER_BOUND('',#2574,.T.);
#1680=FACE_OUTER_BOUND('',#2575,.T.);
#1681=FACE_OUTER_BOUND('',#2577,.T.);
#1682=FACE_OUTER_BOUND('',#2579,.T.);
#1683=FACE_OUTER_BOUND('',#2580,.T.);
#1684=FACE_OUTER_BOUND('',#2581,.T.);
#1685=FACE_OUTER_BOUND('',#2582,.T.);
#1686=FACE_OUTER_BOUND('',#2583,.T.);
#1687=FACE_OUTER_BOUND('',#2584,.T.);
#1688=FACE_OUTER_BOUND('',#2585,.T.);
#1689=FACE_OUTER_BOUND('',#2586,.T.);
#1690=FACE_OUTER_BOUND('',#2587,.T.);
#1691=FACE_OUTER_BOUND('',#2588,.T.);
#1692=FACE_OUTER_BOUND('',#2589,.T.);
#1693=FACE_OUTER_BOUND('',#2590,.T.);
#1694=FACE_OUTER_BOUND('',#2591,.T.);
#1695=FACE_OUTER_BOUND('',#2592,.T.);
#1696=FACE_OUTER_BOUND('',#2593,.T.);
#1697=FACE_OUTER_BOUND('',#2594,.T.);
#1698=FACE_OUTER_BOUND('',#2595,.T.);
#1699=FACE_OUTER_BOUND('',#2596,.T.);
#1700=FACE_OUTER_BOUND('',#2597,.T.);
#1701=FACE_OUTER_BOUND('',#2598,.T.);
#1702=FACE_OUTER_BOUND('',#2599,.T.);
#1703=FACE_OUTER_BOUND('',#2600,.T.);
#1704=FACE_OUTER_BOUND('',#2601,.T.);
#1705=FACE_OUTER_BOUND('',#2602,.T.);
#1706=FACE_OUTER_BOUND('',#2603,.T.);
#1707=FACE_OUTER_BOUND('',#2604,.T.);
#1708=FACE_OUTER_BOUND('',#2605,.T.);
#1709=FACE_OUTER_BOUND('',#2612,.T.);
#1710=FACE_OUTER_BOUND('',#2619,.T.);
#1711=FACE_OUTER_BOUND('',#2620,.T.);
#1712=FACE_OUTER_BOUND('',#2621,.T.);
#1713=FACE_OUTER_BOUND('',#2622,.T.);
#1714=FACE_OUTER_BOUND('',#2623,.T.);
#1715=FACE_OUTER_BOUND('',#2624,.T.);
#1716=FACE_OUTER_BOUND('',#2625,.T.);
#1717=FACE_OUTER_BOUND('',#2626,.T.);
#1718=FACE_OUTER_BOUND('',#2627,.T.);
#1719=FACE_OUTER_BOUND('',#2628,.T.);
#1720=FACE_OUTER_BOUND('',#2629,.T.);
#1721=FACE_OUTER_BOUND('',#2630,.T.);
#1722=FACE_OUTER_BOUND('',#2631,.T.);
#1723=FACE_OUTER_BOUND('',#2632,.T.);
#1724=FACE_OUTER_BOUND('',#2638,.T.);
#1725=FACE_OUTER_BOUND('',#2644,.T.);
#1726=FACE_OUTER_BOUND('',#2645,.T.);
#1727=FACE_OUTER_BOUND('',#2646,.T.);
#1728=FACE_OUTER_BOUND('',#2647,.T.);
#1729=FACE_OUTER_BOUND('',#2648,.T.);
#1730=FACE_OUTER_BOUND('',#2649,.T.);
#1731=FACE_OUTER_BOUND('',#2650,.T.);
#1732=FACE_OUTER_BOUND('',#2651,.T.);
#1733=FACE_OUTER_BOUND('',#2652,.T.);
#1734=FACE_OUTER_BOUND('',#2653,.T.);
#1735=FACE_OUTER_BOUND('',#2659,.T.);
#1736=FACE_OUTER_BOUND('',#2665,.T.);
#1737=FACE_OUTER_BOUND('',#2666,.T.);
#1738=FACE_OUTER_BOUND('',#2667,.T.);
#1739=FACE_OUTER_BOUND('',#2668,.T.);
#1740=FACE_OUTER_BOUND('',#2669,.T.);
#1741=FACE_OUTER_BOUND('',#2670,.T.);
#1742=FACE_OUTER_BOUND('',#2671,.T.);
#1743=FACE_OUTER_BOUND('',#2672,.T.);
#1744=FACE_OUTER_BOUND('',#2673,.T.);
#1745=FACE_OUTER_BOUND('',#2674,.T.);
#1746=FACE_OUTER_BOUND('',#2675,.T.);
#1747=FACE_OUTER_BOUND('',#2676,.T.);
#1748=FACE_OUTER_BOUND('',#2677,.T.);
#1749=FACE_OUTER_BOUND('',#2678,.T.);
#1750=FACE_OUTER_BOUND('',#2679,.T.);
#1751=FACE_OUTER_BOUND('',#2680,.T.);
#1752=FACE_OUTER_BOUND('',#2681,.T.);
#1753=FACE_OUTER_BOUND('',#2682,.T.);
#1754=FACE_OUTER_BOUND('',#2683,.T.);
#1755=FACE_OUTER_BOUND('',#2684,.T.);
#1756=FACE_OUTER_BOUND('',#2685,.T.);
#1757=FACE_OUTER_BOUND('',#2686,.T.);
#1758=FACE_OUTER_BOUND('',#2687,.T.);
#1759=FACE_OUTER_BOUND('',#2688,.T.);
#1760=FACE_OUTER_BOUND('',#2689,.T.);
#1761=FACE_OUTER_BOUND('',#2690,.T.);
#1762=FACE_OUTER_BOUND('',#2691,.T.);
#1763=FACE_OUTER_BOUND('',#2692,.T.);
#1764=FACE_OUTER_BOUND('',#2693,.T.);
#1765=FACE_OUTER_BOUND('',#2694,.T.);
#1766=FACE_OUTER_BOUND('',#2695,.T.);
#1767=FACE_OUTER_BOUND('',#2696,.T.);
#1768=FACE_OUTER_BOUND('',#2697,.T.);
#1769=FACE_OUTER_BOUND('',#2698,.T.);
#1770=FACE_OUTER_BOUND('',#2699,.T.);
#1771=FACE_OUTER_BOUND('',#2700,.T.);
#1772=FACE_OUTER_BOUND('',#2701,.T.);
#1773=FACE_OUTER_BOUND('',#2702,.T.);
#1774=FACE_OUTER_BOUND('',#2703,.T.);
#1775=FACE_OUTER_BOUND('',#2704,.T.);
#1776=FACE_OUTER_BOUND('',#2705,.T.);
#1777=FACE_OUTER_BOUND('',#2724,.T.);
#1778=FACE_OUTER_BOUND('',#2743,.T.);
#1779=FACE_OUTER_BOUND('',#2744,.T.);
#1780=FACE_OUTER_BOUND('',#2745,.T.);
#1781=FACE_OUTER_BOUND('',#2747,.T.);
#1782=FACE_OUTER_BOUND('',#2749,.T.);
#1783=FACE_OUTER_BOUND('',#2750,.T.);
#1784=FACE_OUTER_BOUND('',#2751,.T.);
#1785=FACE_OUTER_BOUND('',#2753,.T.);
#1786=FACE_OUTER_BOUND('',#2755,.T.);
#1787=FACE_OUTER_BOUND('',#2756,.T.);
#1788=FACE_OUTER_BOUND('',#2757,.T.);
#1789=FACE_OUTER_BOUND('',#2758,.T.);
#1790=FACE_OUTER_BOUND('',#2759,.T.);
#1791=FACE_OUTER_BOUND('',#2760,.T.);
#1792=FACE_OUTER_BOUND('',#2761,.T.);
#1793=FACE_OUTER_BOUND('',#2762,.T.);
#1794=FACE_OUTER_BOUND('',#2763,.T.);
#1795=FACE_OUTER_BOUND('',#2764,.T.);
#1796=FACE_OUTER_BOUND('',#2765,.T.);
#1797=FACE_OUTER_BOUND('',#2766,.T.);
#1798=FACE_OUTER_BOUND('',#2767,.T.);
#1799=FACE_OUTER_BOUND('',#2768,.T.);
#1800=FACE_OUTER_BOUND('',#2769,.T.);
#1801=FACE_OUTER_BOUND('',#2783,.T.);
#1802=FACE_OUTER_BOUND('',#2797,.T.);
#1803=FACE_OUTER_BOUND('',#2798,.T.);
#1804=FACE_OUTER_BOUND('',#2799,.T.);
#1805=FACE_OUTER_BOUND('',#2800,.T.);
#1806=FACE_OUTER_BOUND('',#2801,.T.);
#1807=FACE_OUTER_BOUND('',#2802,.T.);
#1808=FACE_OUTER_BOUND('',#2803,.T.);
#1809=FACE_OUTER_BOUND('',#2809,.T.);
#1810=FACE_OUTER_BOUND('',#2815,.T.);
#1811=FACE_OUTER_BOUND('',#2816,.T.);
#1812=FACE_OUTER_BOUND('',#2817,.T.);
#1813=FACE_OUTER_BOUND('',#2818,.T.);
#1814=FACE_OUTER_BOUND('',#2819,.T.);
#1815=FACE_OUTER_BOUND('',#2820,.T.);
#1816=FACE_OUTER_BOUND('',#2821,.T.);
#1817=FACE_OUTER_BOUND('',#2822,.T.);
#1818=FACE_OUTER_BOUND('',#2823,.T.);
#1819=FACE_OUTER_BOUND('',#2824,.T.);
#1820=FACE_OUTER_BOUND('',#2825,.T.);
#1821=FACE_OUTER_BOUND('',#2826,.T.);
#1822=FACE_OUTER_BOUND('',#2827,.T.);
#1823=FACE_OUTER_BOUND('',#2828,.T.);
#1824=FACE_OUTER_BOUND('',#2829,.T.);
#1825=FACE_OUTER_BOUND('',#2830,.T.);
#1826=FACE_OUTER_BOUND('',#2831,.T.);
#1827=FACE_OUTER_BOUND('',#2832,.T.);
#1828=FACE_OUTER_BOUND('',#2833,.T.);
#1829=FACE_OUTER_BOUND('',#2834,.T.);
#1830=FACE_OUTER_BOUND('',#2835,.T.);
#1831=FACE_OUTER_BOUND('',#2836,.T.);
#1832=FACE_OUTER_BOUND('',#2837,.T.);
#1833=FACE_OUTER_BOUND('',#2838,.T.);
#1834=FACE_OUTER_BOUND('',#2839,.T.);
#1835=FACE_OUTER_BOUND('',#2840,.T.);
#1836=FACE_OUTER_BOUND('',#2841,.T.);
#1837=FACE_OUTER_BOUND('',#2842,.T.);
#1838=FACE_OUTER_BOUND('',#2843,.T.);
#1839=FACE_OUTER_BOUND('',#2844,.T.);
#1840=FACE_OUTER_BOUND('',#2845,.T.);
#1841=FACE_OUTER_BOUND('',#2846,.T.);
#1842=FACE_OUTER_BOUND('',#2847,.T.);
#1843=FACE_OUTER_BOUND('',#2848,.T.);
#1844=FACE_OUTER_BOUND('',#2849,.T.);
#1845=FACE_OUTER_BOUND('',#2850,.T.);
#1846=FACE_OUTER_BOUND('',#2851,.T.);
#1847=FACE_OUTER_BOUND('',#2852,.T.);
#1848=FACE_OUTER_BOUND('',#2853,.T.);
#1849=FACE_OUTER_BOUND('',#2854,.T.);
#1850=FACE_OUTER_BOUND('',#2855,.T.);
#1851=FACE_OUTER_BOUND('',#2857,.T.);
#1852=FACE_OUTER_BOUND('',#2859,.T.);
#1853=FACE_OUTER_BOUND('',#2860,.T.);
#1854=FACE_OUTER_BOUND('',#2862,.T.);
#1855=FACE_OUTER_BOUND('',#2864,.T.);
#1856=FACE_OUTER_BOUND('',#2865,.T.);
#1857=FACE_OUTER_BOUND('',#2866,.T.);
#1858=FACE_OUTER_BOUND('',#2867,.T.);
#1859=FACE_OUTER_BOUND('',#2868,.T.);
#1860=FACE_OUTER_BOUND('',#2869,.T.);
#1861=FACE_OUTER_BOUND('',#2870,.T.);
#1862=FACE_OUTER_BOUND('',#2871,.T.);
#1863=FACE_OUTER_BOUND('',#2872,.T.);
#1864=FACE_OUTER_BOUND('',#2873,.T.);
#1865=FACE_OUTER_BOUND('',#2874,.T.);
#1866=FACE_OUTER_BOUND('',#2875,.T.);
#1867=FACE_OUTER_BOUND('',#2876,.T.);
#1868=FACE_OUTER_BOUND('',#2877,.T.);
#1869=FACE_OUTER_BOUND('',#2879,.T.);
#1870=FACE_OUTER_BOUND('',#2881,.T.);
#1871=FACE_OUTER_BOUND('',#2882,.T.);
#1872=FACE_OUTER_BOUND('',#2884,.T.);
#1873=FACE_OUTER_BOUND('',#2886,.T.);
#1874=FACE_OUTER_BOUND('',#2887,.T.);
#1875=FACE_OUTER_BOUND('',#2888,.T.);
#1876=FACE_OUTER_BOUND('',#2889,.T.);
#1877=FACE_OUTER_BOUND('',#2890,.T.);
#1878=FACE_OUTER_BOUND('',#2891,.T.);
#1879=FACE_OUTER_BOUND('',#2892,.T.);
#1880=FACE_OUTER_BOUND('',#2893,.T.);
#1881=FACE_OUTER_BOUND('',#2894,.T.);
#1882=FACE_OUTER_BOUND('',#2895,.T.);
#1883=FACE_OUTER_BOUND('',#2896,.T.);
#1884=FACE_OUTER_BOUND('',#2897,.T.);
#1885=FACE_OUTER_BOUND('',#2898,.T.);
#1886=FACE_OUTER_BOUND('',#2899,.T.);
#1887=FACE_OUTER_BOUND('',#2900,.T.);
#1888=FACE_OUTER_BOUND('',#2901,.T.);
#1889=FACE_OUTER_BOUND('',#2902,.T.);
#1890=FACE_OUTER_BOUND('',#2903,.T.);
#1891=FACE_OUTER_BOUND('',#2904,.T.);
#1892=FACE_OUTER_BOUND('',#2905,.T.);
#1893=FACE_OUTER_BOUND('',#2906,.T.);
#1894=FACE_OUTER_BOUND('',#2907,.T.);
#1895=FACE_OUTER_BOUND('',#2908,.T.);
#1896=FACE_OUTER_BOUND('',#2909,.T.);
#1897=FACE_OUTER_BOUND('',#2910,.T.);
#1898=FACE_OUTER_BOUND('',#2911,.T.);
#1899=FACE_OUTER_BOUND('',#2912,.T.);
#1900=FACE_OUTER_BOUND('',#2913,.T.);
#1901=FACE_OUTER_BOUND('',#2914,.T.);
#1902=FACE_OUTER_BOUND('',#2916,.T.);
#1903=FACE_OUTER_BOUND('',#2918,.T.);
#1904=FACE_OUTER_BOUND('',#2919,.T.);
#1905=FACE_OUTER_BOUND('',#2920,.T.);
#1906=FACE_OUTER_BOUND('',#2921,.T.);
#1907=FACE_OUTER_BOUND('',#2922,.T.);
#1908=FACE_OUTER_BOUND('',#2923,.T.);
#1909=FACE_OUTER_BOUND('',#2924,.T.);
#1910=FACE_OUTER_BOUND('',#2925,.T.);
#1911=FACE_OUTER_BOUND('',#2927,.T.);
#1912=FACE_OUTER_BOUND('',#2929,.T.);
#1913=FACE_OUTER_BOUND('',#2930,.T.);
#1914=FACE_OUTER_BOUND('',#2931,.T.);
#1915=FACE_OUTER_BOUND('',#2932,.T.);
#1916=FACE_OUTER_BOUND('',#2933,.T.);
#1917=FACE_OUTER_BOUND('',#2934,.T.);
#1918=FACE_OUTER_BOUND('',#2935,.T.);
#1919=FACE_OUTER_BOUND('',#2936,.T.);
#1920=FACE_OUTER_BOUND('',#2937,.T.);
#1921=FACE_OUTER_BOUND('',#2938,.T.);
#1922=FACE_OUTER_BOUND('',#2939,.T.);
#1923=FACE_OUTER_BOUND('',#2940,.T.);
#1924=FACE_OUTER_BOUND('',#2941,.T.);
#1925=FACE_OUTER_BOUND('',#2942,.T.);
#1926=FACE_OUTER_BOUND('',#2943,.T.);
#1927=FACE_OUTER_BOUND('',#2944,.T.);
#1928=FACE_OUTER_BOUND('',#2945,.T.);
#1929=FACE_OUTER_BOUND('',#2946,.T.);
#1930=FACE_OUTER_BOUND('',#2947,.T.);
#1931=FACE_OUTER_BOUND('',#2948,.T.);
#1932=FACE_OUTER_BOUND('',#2949,.T.);
#1933=FACE_OUTER_BOUND('',#2950,.T.);
#1934=FACE_OUTER_BOUND('',#2951,.T.);
#1935=FACE_OUTER_BOUND('',#2952,.T.);
#1936=FACE_OUTER_BOUND('',#2954,.T.);
#1937=FACE_OUTER_BOUND('',#2956,.T.);
#1938=FACE_OUTER_BOUND('',#2957,.T.);
#1939=FACE_OUTER_BOUND('',#2958,.T.);
#1940=FACE_OUTER_BOUND('',#2959,.T.);
#1941=FACE_OUTER_BOUND('',#2960,.T.);
#1942=FACE_OUTER_BOUND('',#2961,.T.);
#1943=FACE_OUTER_BOUND('',#2962,.T.);
#1944=FACE_OUTER_BOUND('',#2963,.T.);
#1945=FACE_OUTER_BOUND('',#2965,.T.);
#1946=FACE_OUTER_BOUND('',#2967,.T.);
#1947=FACE_OUTER_BOUND('',#2968,.T.);
#1948=FACE_OUTER_BOUND('',#2969,.T.);
#1949=FACE_OUTER_BOUND('',#2970,.T.);
#1950=FACE_OUTER_BOUND('',#2971,.T.);
#1951=FACE_OUTER_BOUND('',#2972,.T.);
#1952=FACE_OUTER_BOUND('',#2973,.T.);
#1953=FACE_OUTER_BOUND('',#2974,.T.);
#1954=FACE_OUTER_BOUND('',#2975,.T.);
#1955=FACE_OUTER_BOUND('',#2976,.T.);
#1956=FACE_OUTER_BOUND('',#2977,.T.);
#1957=FACE_OUTER_BOUND('',#2978,.T.);
#1958=FACE_OUTER_BOUND('',#2979,.T.);
#1959=FACE_OUTER_BOUND('',#2980,.T.);
#1960=FACE_OUTER_BOUND('',#2981,.T.);
#1961=FACE_OUTER_BOUND('',#2982,.T.);
#1962=FACE_OUTER_BOUND('',#2983,.T.);
#1963=FACE_OUTER_BOUND('',#2984,.T.);
#1964=FACE_OUTER_BOUND('',#2985,.T.);
#1965=FACE_OUTER_BOUND('',#2986,.T.);
#1966=FACE_OUTER_BOUND('',#2988,.T.);
#1967=FACE_OUTER_BOUND('',#2989,.T.);
#1968=FACE_OUTER_BOUND('',#2990,.T.);
#1969=FACE_OUTER_BOUND('',#2991,.T.);
#1970=FACE_OUTER_BOUND('',#2992,.T.);
#1971=FACE_OUTER_BOUND('',#2993,.T.);
#1972=FACE_OUTER_BOUND('',#2994,.T.);
#1973=FACE_OUTER_BOUND('',#2995,.T.);
#1974=FACE_OUTER_BOUND('',#2996,.T.);
#1975=FACE_OUTER_BOUND('',#2997,.T.);
#1976=FACE_OUTER_BOUND('',#2998,.T.);
#1977=FACE_OUTER_BOUND('',#2999,.T.);
#1978=FACE_OUTER_BOUND('',#3000,.T.);
#1979=FACE_OUTER_BOUND('',#3001,.T.);
#1980=FACE_OUTER_BOUND('',#3002,.T.);
#1981=FACE_OUTER_BOUND('',#3003,.T.);
#1982=FACE_OUTER_BOUND('',#3004,.T.);
#1983=FACE_OUTER_BOUND('',#3006,.T.);
#1984=FACE_OUTER_BOUND('',#3007,.T.);
#1985=FACE_OUTER_BOUND('',#3008,.T.);
#1986=FACE_OUTER_BOUND('',#3009,.T.);
#1987=FACE_OUTER_BOUND('',#3010,.T.);
#1988=FACE_OUTER_BOUND('',#3011,.T.);
#1989=FACE_OUTER_BOUND('',#3012,.T.);
#1990=FACE_OUTER_BOUND('',#3013,.T.);
#1991=FACE_OUTER_BOUND('',#3014,.T.);
#1992=FACE_OUTER_BOUND('',#3015,.T.);
#1993=FACE_OUTER_BOUND('',#3016,.T.);
#1994=FACE_OUTER_BOUND('',#3017,.T.);
#1995=FACE_OUTER_BOUND('',#3018,.T.);
#1996=FACE_OUTER_BOUND('',#3019,.T.);
#1997=FACE_OUTER_BOUND('',#3020,.T.);
#1998=FACE_OUTER_BOUND('',#3021,.T.);
#1999=FACE_OUTER_BOUND('',#3022,.T.);
#2000=FACE_OUTER_BOUND('',#3023,.T.);
#2001=FACE_OUTER_BOUND('',#3024,.T.);
#2002=FACE_OUTER_BOUND('',#3026,.T.);
#2003=FACE_OUTER_BOUND('',#3028,.T.);
#2004=FACE_OUTER_BOUND('',#3029,.T.);
#2005=FACE_OUTER_BOUND('',#3030,.T.);
#2006=FACE_OUTER_BOUND('',#3031,.T.);
#2007=FACE_OUTER_BOUND('',#3032,.T.);
#2008=FACE_OUTER_BOUND('',#3033,.T.);
#2009=FACE_OUTER_BOUND('',#3034,.T.);
#2010=FACE_OUTER_BOUND('',#3035,.T.);
#2011=FACE_OUTER_BOUND('',#3036,.T.);
#2012=FACE_OUTER_BOUND('',#3037,.T.);
#2013=FACE_OUTER_BOUND('',#3038,.T.);
#2014=FACE_OUTER_BOUND('',#3039,.T.);
#2015=FACE_OUTER_BOUND('',#3040,.T.);
#2016=FACE_OUTER_BOUND('',#3041,.T.);
#2017=FACE_OUTER_BOUND('',#3042,.T.);
#2018=FACE_OUTER_BOUND('',#3043,.T.);
#2019=FACE_OUTER_BOUND('',#3044,.T.);
#2020=FACE_OUTER_BOUND('',#3045,.T.);
#2021=FACE_OUTER_BOUND('',#3046,.T.);
#2022=FACE_OUTER_BOUND('',#3047,.T.);
#2023=FACE_OUTER_BOUND('',#3048,.T.);
#2024=FACE_OUTER_BOUND('',#3049,.T.);
#2025=FACE_OUTER_BOUND('',#3050,.T.);
#2026=FACE_OUTER_BOUND('',#3051,.T.);
#2027=FACE_OUTER_BOUND('',#3052,.T.);
#2028=FACE_OUTER_BOUND('',#3053,.T.);
#2029=FACE_OUTER_BOUND('',#3054,.T.);
#2030=FACE_OUTER_BOUND('',#3055,.T.);
#2031=FACE_OUTER_BOUND('',#3056,.T.);
#2032=FACE_OUTER_BOUND('',#3057,.T.);
#2033=FACE_OUTER_BOUND('',#3058,.T.);
#2034=FACE_OUTER_BOUND('',#3059,.T.);
#2035=FACE_OUTER_BOUND('',#3060,.T.);
#2036=FACE_OUTER_BOUND('',#3061,.T.);
#2037=FACE_OUTER_BOUND('',#3062,.T.);
#2038=FACE_OUTER_BOUND('',#3063,.T.);
#2039=FACE_OUTER_BOUND('',#3064,.T.);
#2040=FACE_OUTER_BOUND('',#3065,.T.);
#2041=FACE_OUTER_BOUND('',#3066,.T.);
#2042=FACE_OUTER_BOUND('',#3067,.T.);
#2043=FACE_OUTER_BOUND('',#3068,.T.);
#2044=FACE_OUTER_BOUND('',#3069,.T.);
#2045=FACE_OUTER_BOUND('',#3070,.T.);
#2046=FACE_OUTER_BOUND('',#3071,.T.);
#2047=FACE_OUTER_BOUND('',#3072,.T.);
#2048=FACE_OUTER_BOUND('',#3073,.T.);
#2049=FACE_OUTER_BOUND('',#3074,.T.);
#2050=FACE_OUTER_BOUND('',#3075,.T.);
#2051=FACE_OUTER_BOUND('',#3076,.T.);
#2052=FACE_OUTER_BOUND('',#3077,.T.);
#2053=FACE_OUTER_BOUND('',#3078,.T.);
#2054=FACE_OUTER_BOUND('',#3079,.T.);
#2055=FACE_OUTER_BOUND('',#3080,.T.);
#2056=FACE_OUTER_BOUND('',#3081,.T.);
#2057=FACE_OUTER_BOUND('',#3082,.T.);
#2058=FACE_OUTER_BOUND('',#3083,.T.);
#2059=FACE_OUTER_BOUND('',#3084,.T.);
#2060=FACE_OUTER_BOUND('',#3085,.T.);
#2061=FACE_OUTER_BOUND('',#3086,.T.);
#2062=FACE_OUTER_BOUND('',#3087,.T.);
#2063=FACE_OUTER_BOUND('',#3088,.T.);
#2064=FACE_OUTER_BOUND('',#3089,.T.);
#2065=FACE_OUTER_BOUND('',#3091,.T.);
#2066=FACE_OUTER_BOUND('',#3093,.T.);
#2067=FACE_OUTER_BOUND('',#3094,.T.);
#2068=FACE_OUTER_BOUND('',#3095,.T.);
#2069=FACE_OUTER_BOUND('',#3096,.T.);
#2070=FACE_OUTER_BOUND('',#3097,.T.);
#2071=FACE_OUTER_BOUND('',#3098,.T.);
#2072=FACE_OUTER_BOUND('',#3099,.T.);
#2073=FACE_OUTER_BOUND('',#3100,.T.);
#2074=FACE_OUTER_BOUND('',#3101,.T.);
#2075=FACE_OUTER_BOUND('',#3102,.T.);
#2076=FACE_OUTER_BOUND('',#3103,.T.);
#2077=FACE_OUTER_BOUND('',#3104,.T.);
#2078=FACE_OUTER_BOUND('',#3105,.T.);
#2079=FACE_OUTER_BOUND('',#3106,.T.);
#2080=FACE_OUTER_BOUND('',#3107,.T.);
#2081=FACE_OUTER_BOUND('',#3108,.T.);
#2082=FACE_OUTER_BOUND('',#3109,.T.);
#2083=FACE_OUTER_BOUND('',#3110,.T.);
#2084=FACE_OUTER_BOUND('',#3111,.T.);
#2085=FACE_OUTER_BOUND('',#3112,.T.);
#2086=FACE_OUTER_BOUND('',#3113,.T.);
#2087=FACE_OUTER_BOUND('',#3114,.T.);
#2088=FACE_OUTER_BOUND('',#3115,.T.);
#2089=FACE_OUTER_BOUND('',#3116,.T.);
#2090=FACE_OUTER_BOUND('',#3117,.T.);
#2091=FACE_OUTER_BOUND('',#3118,.T.);
#2092=FACE_OUTER_BOUND('',#3119,.T.);
#2093=FACE_OUTER_BOUND('',#3120,.T.);
#2094=FACE_OUTER_BOUND('',#3121,.T.);
#2095=FACE_OUTER_BOUND('',#3122,.T.);
#2096=FACE_OUTER_BOUND('',#3123,.T.);
#2097=FACE_OUTER_BOUND('',#3124,.T.);
#2098=FACE_OUTER_BOUND('',#3125,.T.);
#2099=FACE_OUTER_BOUND('',#3126,.T.);
#2100=FACE_OUTER_BOUND('',#3127,.T.);
#2101=FACE_OUTER_BOUND('',#3128,.T.);
#2102=FACE_OUTER_BOUND('',#3129,.T.);
#2103=FACE_OUTER_BOUND('',#3130,.T.);
#2104=FACE_OUTER_BOUND('',#3132,.T.);
#2105=FACE_OUTER_BOUND('',#3134,.T.);
#2106=FACE_OUTER_BOUND('',#3135,.T.);
#2107=FACE_OUTER_BOUND('',#3136,.T.);
#2108=FACE_OUTER_BOUND('',#3137,.T.);
#2109=FACE_OUTER_BOUND('',#3138,.T.);
#2110=FACE_OUTER_BOUND('',#3139,.T.);
#2111=FACE_OUTER_BOUND('',#3140,.T.);
#2112=FACE_OUTER_BOUND('',#3141,.T.);
#2113=FACE_OUTER_BOUND('',#3142,.T.);
#2114=FACE_OUTER_BOUND('',#3143,.T.);
#2115=FACE_OUTER_BOUND('',#3144,.T.);
#2116=FACE_OUTER_BOUND('',#3145,.T.);
#2117=FACE_OUTER_BOUND('',#3146,.T.);
#2118=FACE_OUTER_BOUND('',#3147,.T.);
#2119=FACE_OUTER_BOUND('',#3148,.T.);
#2120=FACE_OUTER_BOUND('',#3149,.T.);
#2121=FACE_OUTER_BOUND('',#3150,.T.);
#2122=FACE_OUTER_BOUND('',#3151,.T.);
#2123=FACE_OUTER_BOUND('',#3152,.T.);
#2124=FACE_OUTER_BOUND('',#3153,.T.);
#2125=FACE_OUTER_BOUND('',#3154,.T.);
#2126=FACE_OUTER_BOUND('',#3155,.T.);
#2127=FACE_OUTER_BOUND('',#3156,.T.);
#2128=FACE_OUTER_BOUND('',#3157,.T.);
#2129=FACE_OUTER_BOUND('',#3159,.T.);
#2130=FACE_OUTER_BOUND('',#3161,.T.);
#2131=FACE_OUTER_BOUND('',#3162,.T.);
#2132=FACE_OUTER_BOUND('',#3163,.T.);
#2133=FACE_OUTER_BOUND('',#3164,.T.);
#2134=FACE_OUTER_BOUND('',#3165,.T.);
#2135=FACE_OUTER_BOUND('',#3166,.T.);
#2136=FACE_OUTER_BOUND('',#3167,.T.);
#2137=FACE_OUTER_BOUND('',#3168,.T.);
#2138=FACE_OUTER_BOUND('',#3170,.T.);
#2139=FACE_OUTER_BOUND('',#3172,.T.);
#2140=FACE_OUTER_BOUND('',#3173,.T.);
#2141=FACE_OUTER_BOUND('',#3174,.T.);
#2142=FACE_OUTER_BOUND('',#3175,.T.);
#2143=FACE_OUTER_BOUND('',#3176,.T.);
#2144=FACE_OUTER_BOUND('',#3177,.T.);
#2145=FACE_OUTER_BOUND('',#3178,.T.);
#2146=FACE_OUTER_BOUND('',#3179,.T.);
#2147=FACE_OUTER_BOUND('',#3181,.T.);
#2148=FACE_OUTER_BOUND('',#3183,.T.);
#2149=FACE_OUTER_BOUND('',#3184,.T.);
#2150=FACE_OUTER_BOUND('',#3185,.T.);
#2151=FACE_OUTER_BOUND('',#3186,.T.);
#2152=FACE_OUTER_BOUND('',#3187,.T.);
#2153=FACE_OUTER_BOUND('',#3188,.T.);
#2154=FACE_OUTER_BOUND('',#3189,.T.);
#2155=FACE_OUTER_BOUND('',#3190,.T.);
#2156=FACE_OUTER_BOUND('',#3191,.T.);
#2157=FACE_OUTER_BOUND('',#3192,.T.);
#2158=FACE_OUTER_BOUND('',#3193,.T.);
#2159=FACE_OUTER_BOUND('',#3194,.T.);
#2160=FACE_OUTER_BOUND('',#3200,.T.);
#2161=FACE_OUTER_BOUND('',#3206,.T.);
#2162=FACE_OUTER_BOUND('',#3207,.T.);
#2163=FACE_OUTER_BOUND('',#3208,.T.);
#2164=FACE_OUTER_BOUND('',#3209,.T.);
#2165=FACE_OUTER_BOUND('',#3210,.T.);
#2166=FACE_OUTER_BOUND('',#3211,.T.);
#2167=FACE_OUTER_BOUND('',#3212,.T.);
#2168=FACE_OUTER_BOUND('',#3213,.T.);
#2169=FACE_OUTER_BOUND('',#3214,.T.);
#2170=FACE_OUTER_BOUND('',#3215,.T.);
#2171=FACE_OUTER_BOUND('',#3216,.T.);
#2172=FACE_OUTER_BOUND('',#3217,.T.);
#2173=FACE_OUTER_BOUND('',#3218,.T.);
#2174=FACE_OUTER_BOUND('',#3219,.T.);
#2175=FACE_OUTER_BOUND('',#3220,.T.);
#2176=FACE_OUTER_BOUND('',#3221,.T.);
#2177=FACE_OUTER_BOUND('',#3222,.T.);
#2178=FACE_OUTER_BOUND('',#3223,.T.);
#2179=FACE_OUTER_BOUND('',#3224,.T.);
#2180=FACE_OUTER_BOUND('',#3225,.T.);
#2181=FACE_OUTER_BOUND('',#3226,.T.);
#2182=FACE_OUTER_BOUND('',#3227,.T.);
#2183=FACE_OUTER_BOUND('',#3228,.T.);
#2184=FACE_OUTER_BOUND('',#3229,.T.);
#2185=FACE_OUTER_BOUND('',#3230,.T.);
#2186=FACE_OUTER_BOUND('',#3231,.T.);
#2187=FACE_OUTER_BOUND('',#3232,.T.);
#2188=FACE_OUTER_BOUND('',#3233,.T.);
#2189=FACE_OUTER_BOUND('',#3234,.T.);
#2190=FACE_OUTER_BOUND('',#3235,.T.);
#2191=FACE_OUTER_BOUND('',#3236,.T.);
#2192=FACE_OUTER_BOUND('',#3237,.T.);
#2193=FACE_OUTER_BOUND('',#3241,.T.);
#2194=FACE_OUTER_BOUND('',#3245,.T.);
#2195=FACE_OUTER_BOUND('',#3246,.T.);
#2196=FACE_OUTER_BOUND('',#3247,.T.);
#2197=FACE_OUTER_BOUND('',#3248,.T.);
#2198=FACE_OUTER_BOUND('',#3249,.T.);
#2199=FACE_OUTER_BOUND('',#3250,.T.);
#2200=FACE_OUTER_BOUND('',#3251,.T.);
#2201=FACE_OUTER_BOUND('',#3252,.T.);
#2202=FACE_OUTER_BOUND('',#3256,.T.);
#2203=FACE_OUTER_BOUND('',#3260,.T.);
#2204=FACE_OUTER_BOUND('',#3261,.T.);
#2205=FACE_OUTER_BOUND('',#3262,.T.);
#2206=FACE_OUTER_BOUND('',#3263,.T.);
#2207=FACE_OUTER_BOUND('',#3264,.T.);
#2208=FACE_OUTER_BOUND('',#3265,.T.);
#2209=FACE_OUTER_BOUND('',#3266,.T.);
#2210=FACE_OUTER_BOUND('',#3267,.T.);
#2211=FACE_OUTER_BOUND('',#3271,.T.);
#2212=FACE_OUTER_BOUND('',#3275,.T.);
#2213=FACE_OUTER_BOUND('',#3276,.T.);
#2214=FACE_OUTER_BOUND('',#3277,.T.);
#2215=FACE_OUTER_BOUND('',#3278,.T.);
#2216=FACE_OUTER_BOUND('',#3279,.T.);
#2217=FACE_OUTER_BOUND('',#3280,.T.);
#2218=FACE_OUTER_BOUND('',#3281,.T.);
#2219=FACE_OUTER_BOUND('',#3282,.T.);
#2220=FACE_OUTER_BOUND('',#3286,.T.);
#2221=FACE_OUTER_BOUND('',#3290,.T.);
#2222=FACE_OUTER_BOUND('',#3291,.T.);
#2223=FACE_OUTER_BOUND('',#3292,.T.);
#2224=FACE_OUTER_BOUND('',#3293,.T.);
#2225=FACE_OUTER_BOUND('',#3294,.T.);
#2226=FACE_OUTER_BOUND('',#3295,.T.);
#2227=FACE_OUTER_BOUND('',#3296,.T.);
#2228=FACE_OUTER_BOUND('',#3297,.T.);
#2229=FACE_OUTER_BOUND('',#3298,.T.);
#2230=FACE_OUTER_BOUND('',#3299,.T.);
#2231=FACE_OUTER_BOUND('',#3300,.T.);
#2232=FACE_OUTER_BOUND('',#3301,.T.);
#2233=FACE_OUTER_BOUND('',#3302,.T.);
#2234=FACE_OUTER_BOUND('',#3303,.T.);
#2235=FACE_OUTER_BOUND('',#3304,.T.);
#2236=FACE_OUTER_BOUND('',#3305,.T.);
#2237=FACE_OUTER_BOUND('',#3306,.T.);
#2238=FACE_OUTER_BOUND('',#3307,.T.);
#2239=FACE_OUTER_BOUND('',#3308,.T.);
#2240=FACE_OUTER_BOUND('',#3309,.T.);
#2241=FACE_OUTER_BOUND('',#3310,.T.);
#2242=FACE_OUTER_BOUND('',#3311,.T.);
#2243=FACE_OUTER_BOUND('',#3312,.T.);
#2244=FACE_OUTER_BOUND('',#3313,.T.);
#2245=FACE_OUTER_BOUND('',#3314,.T.);
#2246=FACE_OUTER_BOUND('',#3315,.T.);
#2247=FACE_OUTER_BOUND('',#3316,.T.);
#2248=FACE_OUTER_BOUND('',#3317,.T.);
#2249=FACE_OUTER_BOUND('',#3318,.T.);
#2250=FACE_OUTER_BOUND('',#3319,.T.);
#2251=FACE_OUTER_BOUND('',#3320,.T.);
#2252=FACE_OUTER_BOUND('',#3321,.T.);
#2253=FACE_OUTER_BOUND('',#3322,.T.);
#2254=FACE_OUTER_BOUND('',#3323,.T.);
#2255=FACE_OUTER_BOUND('',#3324,.T.);
#2256=FACE_OUTER_BOUND('',#3325,.T.);
#2257=FACE_OUTER_BOUND('',#3326,.T.);
#2258=FACE_OUTER_BOUND('',#3327,.T.);
#2259=FACE_OUTER_BOUND('',#3328,.T.);
#2260=FACE_OUTER_BOUND('',#3333,.T.);
#2261=FACE_OUTER_BOUND('',#3338,.T.);
#2262=FACE_OUTER_BOUND('',#3339,.T.);
#2263=FACE_OUTER_BOUND('',#3340,.T.);
#2264=FACE_OUTER_BOUND('',#3341,.T.);
#2265=FACE_OUTER_BOUND('',#3342,.T.);
#2266=FACE_OUTER_BOUND('',#3343,.T.);
#2267=FACE_OUTER_BOUND('',#3344,.T.);
#2268=FACE_OUTER_BOUND('',#3345,.T.);
#2269=FACE_OUTER_BOUND('',#3346,.T.);
#2270=FACE_OUTER_BOUND('',#3347,.T.);
#2271=FACE_OUTER_BOUND('',#3348,.T.);
#2272=FACE_OUTER_BOUND('',#3349,.T.);
#2273=FACE_OUTER_BOUND('',#3350,.T.);
#2274=FACE_OUTER_BOUND('',#3351,.T.);
#2275=FACE_OUTER_BOUND('',#3352,.T.);
#2276=FACE_OUTER_BOUND('',#3359,.T.);
#2277=FACE_OUTER_BOUND('',#3366,.T.);
#2278=FACE_OUTER_BOUND('',#3367,.T.);
#2279=FACE_OUTER_BOUND('',#3368,.T.);
#2280=FACE_OUTER_BOUND('',#3369,.T.);
#2281=FACE_OUTER_BOUND('',#3370,.T.);
#2282=FACE_OUTER_BOUND('',#3371,.T.);
#2283=FACE_OUTER_BOUND('',#3372,.T.);
#2284=FACE_OUTER_BOUND('',#3373,.T.);
#2285=FACE_OUTER_BOUND('',#3374,.T.);
#2286=FACE_OUTER_BOUND('',#3375,.T.);
#2287=FACE_OUTER_BOUND('',#3376,.T.);
#2288=FACE_OUTER_BOUND('',#3377,.T.);
#2289=FACE_OUTER_BOUND('',#3378,.T.);
#2290=FACE_OUTER_BOUND('',#3379,.T.);
#2291=FACE_OUTER_BOUND('',#3380,.T.);
#2292=FACE_OUTER_BOUND('',#3381,.T.);
#2293=FACE_OUTER_BOUND('',#3382,.T.);
#2294=FACE_OUTER_BOUND('',#3383,.T.);
#2295=FACE_OUTER_BOUND('',#3384,.T.);
#2296=FACE_OUTER_BOUND('',#3385,.T.);
#2297=FACE_OUTER_BOUND('',#3386,.T.);
#2298=FACE_OUTER_BOUND('',#3387,.T.);
#2299=FACE_OUTER_BOUND('',#3388,.T.);
#2300=FACE_OUTER_BOUND('',#3389,.T.);
#2301=FACE_OUTER_BOUND('',#3390,.T.);
#2302=FACE_OUTER_BOUND('',#3391,.T.);
#2303=FACE_OUTER_BOUND('',#3392,.T.);
#2304=FACE_OUTER_BOUND('',#3393,.T.);
#2305=FACE_OUTER_BOUND('',#3394,.T.);
#2306=FACE_OUTER_BOUND('',#3395,.T.);
#2307=FACE_OUTER_BOUND('',#3396,.T.);
#2308=FACE_OUTER_BOUND('',#3397,.T.);
#2309=FACE_OUTER_BOUND('',#3398,.T.);
#2310=FACE_OUTER_BOUND('',#3399,.T.);
#2311=FACE_OUTER_BOUND('',#3400,.T.);
#2312=FACE_OUTER_BOUND('',#3401,.T.);
#2313=FACE_OUTER_BOUND('',#3402,.T.);
#2314=FACE_OUTER_BOUND('',#3403,.T.);
#2315=FACE_OUTER_BOUND('',#3404,.T.);
#2316=FACE_OUTER_BOUND('',#3405,.T.);
#2317=FACE_OUTER_BOUND('',#3406,.T.);
#2318=FACE_OUTER_BOUND('',#3407,.T.);
#2319=FACE_OUTER_BOUND('',#3408,.T.);
#2320=FACE_OUTER_BOUND('',#3409,.T.);
#2321=FACE_OUTER_BOUND('',#3410,.T.);
#2322=FACE_OUTER_BOUND('',#3411,.T.);
#2323=FACE_OUTER_BOUND('',#3412,.T.);
#2324=FACE_OUTER_BOUND('',#3413,.T.);
#2325=FACE_OUTER_BOUND('',#3414,.T.);
#2326=FACE_OUTER_BOUND('',#3415,.T.);
#2327=FACE_OUTER_BOUND('',#3416,.T.);
#2328=FACE_OUTER_BOUND('',#3417,.T.);
#2329=FACE_OUTER_BOUND('',#3418,.T.);
#2330=FACE_OUTER_BOUND('',#3419,.T.);
#2331=FACE_OUTER_BOUND('',#3420,.T.);
#2332=FACE_OUTER_BOUND('',#3421,.T.);
#2333=FACE_OUTER_BOUND('',#3422,.T.);
#2334=FACE_OUTER_BOUND('',#3423,.T.);
#2335=FACE_OUTER_BOUND('',#3424,.T.);
#2336=FACE_OUTER_BOUND('',#3425,.T.);
#2337=FACE_OUTER_BOUND('',#3426,.T.);
#2338=FACE_OUTER_BOUND('',#3427,.T.);
#2339=FACE_OUTER_BOUND('',#3428,.T.);
#2340=FACE_OUTER_BOUND('',#3429,.T.);
#2341=FACE_OUTER_BOUND('',#3430,.T.);
#2342=FACE_OUTER_BOUND('',#3431,.T.);
#2343=FACE_OUTER_BOUND('',#3432,.T.);
#2344=FACE_OUTER_BOUND('',#3433,.T.);
#2345=FACE_OUTER_BOUND('',#3434,.T.);
#2346=FACE_OUTER_BOUND('',#3435,.T.);
#2347=FACE_OUTER_BOUND('',#3436,.T.);
#2348=FACE_OUTER_BOUND('',#3437,.T.);
#2349=FACE_OUTER_BOUND('',#3438,.T.);
#2350=FACE_OUTER_BOUND('',#3439,.T.);
#2351=FACE_OUTER_BOUND('',#3440,.T.);
#2352=FACE_OUTER_BOUND('',#3441,.T.);
#2353=FACE_OUTER_BOUND('',#3442,.T.);
#2354=FACE_OUTER_BOUND('',#3443,.T.);
#2355=FACE_OUTER_BOUND('',#3444,.T.);
#2356=FACE_OUTER_BOUND('',#3445,.T.);
#2357=FACE_OUTER_BOUND('',#3446,.T.);
#2358=FACE_OUTER_BOUND('',#3447,.T.);
#2359=FACE_OUTER_BOUND('',#3448,.T.);
#2360=FACE_OUTER_BOUND('',#3449,.T.);
#2361=FACE_OUTER_BOUND('',#3450,.T.);
#2362=FACE_OUTER_BOUND('',#3451,.T.);
#2363=FACE_OUTER_BOUND('',#3452,.T.);
#2364=FACE_OUTER_BOUND('',#3453,.T.);
#2365=FACE_OUTER_BOUND('',#3454,.T.);
#2366=FACE_OUTER_BOUND('',#3455,.T.);
#2367=FACE_OUTER_BOUND('',#3456,.T.);
#2368=FACE_OUTER_BOUND('',#3457,.T.);
#2369=FACE_OUTER_BOUND('',#3458,.T.);
#2370=FACE_OUTER_BOUND('',#3459,.T.);
#2371=FACE_OUTER_BOUND('',#3460,.T.);
#2372=FACE_OUTER_BOUND('',#3461,.T.);
#2373=FACE_OUTER_BOUND('',#3462,.T.);
#2374=FACE_OUTER_BOUND('',#3463,.T.);
#2375=FACE_OUTER_BOUND('',#3464,.T.);
#2376=FACE_OUTER_BOUND('',#3465,.T.);
#2377=FACE_OUTER_BOUND('',#3466,.T.);
#2378=FACE_OUTER_BOUND('',#3467,.T.);
#2379=FACE_OUTER_BOUND('',#3468,.T.);
#2380=FACE_OUTER_BOUND('',#3469,.T.);
#2381=FACE_OUTER_BOUND('',#3474,.T.);
#2382=FACE_OUTER_BOUND('',#3479,.T.);
#2383=FACE_OUTER_BOUND('',#3480,.T.);
#2384=FACE_OUTER_BOUND('',#3481,.T.);
#2385=FACE_OUTER_BOUND('',#3482,.T.);
#2386=FACE_OUTER_BOUND('',#3483,.T.);
#2387=FACE_OUTER_BOUND('',#3484,.T.);
#2388=FACE_OUTER_BOUND('',#3485,.T.);
#2389=FACE_OUTER_BOUND('',#3486,.T.);
#2390=FACE_OUTER_BOUND('',#3487,.T.);
#2391=FACE_OUTER_BOUND('',#3488,.T.);
#2392=FACE_OUTER_BOUND('',#3489,.T.);
#2393=FACE_OUTER_BOUND('',#3490,.T.);
#2394=FACE_OUTER_BOUND('',#3491,.T.);
#2395=FACE_OUTER_BOUND('',#3492,.T.);
#2396=FACE_OUTER_BOUND('',#3493,.T.);
#2397=FACE_OUTER_BOUND('',#3494,.T.);
#2398=FACE_OUTER_BOUND('',#3495,.T.);
#2399=FACE_OUTER_BOUND('',#3496,.T.);
#2400=FACE_OUTER_BOUND('',#3497,.T.);
#2401=FACE_OUTER_BOUND('',#3498,.T.);
#2402=FACE_OUTER_BOUND('',#3499,.T.);
#2403=FACE_OUTER_BOUND('',#3500,.T.);
#2404=FACE_OUTER_BOUND('',#3501,.T.);
#2405=FACE_OUTER_BOUND('',#3502,.T.);
#2406=FACE_OUTER_BOUND('',#3503,.T.);
#2407=FACE_OUTER_BOUND('',#3504,.T.);
#2408=FACE_OUTER_BOUND('',#3505,.T.);
#2409=FACE_OUTER_BOUND('',#3506,.T.);
#2410=FACE_OUTER_BOUND('',#3507,.T.);
#2411=FACE_OUTER_BOUND('',#3508,.T.);
#2412=FACE_OUTER_BOUND('',#3509,.T.);
#2413=FACE_OUTER_BOUND('',#3510,.T.);
#2414=FACE_OUTER_BOUND('',#3511,.T.);
#2415=FACE_OUTER_BOUND('',#3512,.T.);
#2416=FACE_OUTER_BOUND('',#3513,.T.);
#2417=FACE_OUTER_BOUND('',#3514,.T.);
#2418=FACE_OUTER_BOUND('',#3515,.T.);
#2419=FACE_OUTER_BOUND('',#3516,.T.);
#2420=FACE_OUTER_BOUND('',#3517,.T.);
#2421=FACE_OUTER_BOUND('',#3518,.T.);
#2422=FACE_OUTER_BOUND('',#3519,.T.);
#2423=FACE_OUTER_BOUND('',#3520,.T.);
#2424=FACE_OUTER_BOUND('',#3521,.T.);
#2425=FACE_OUTER_BOUND('',#3522,.T.);
#2426=FACE_OUTER_BOUND('',#3523,.T.);
#2427=FACE_OUTER_BOUND('',#3524,.T.);
#2428=FACE_OUTER_BOUND('',#3525,.T.);
#2429=FACE_OUTER_BOUND('',#3526,.T.);
#2430=FACE_OUTER_BOUND('',#3527,.T.);
#2431=FACE_OUTER_BOUND('',#3528,.T.);
#2432=FACE_OUTER_BOUND('',#3529,.T.);
#2433=FACE_OUTER_BOUND('',#3530,.T.);
#2434=FACE_OUTER_BOUND('',#3531,.T.);
#2435=FACE_OUTER_BOUND('',#3532,.T.);
#2436=FACE_OUTER_BOUND('',#3533,.T.);
#2437=FACE_OUTER_BOUND('',#3534,.T.);
#2438=FACE_OUTER_BOUND('',#3535,.T.);
#2439=FACE_OUTER_BOUND('',#3536,.T.);
#2440=FACE_OUTER_BOUND('',#3537,.T.);
#2441=FACE_OUTER_BOUND('',#3538,.T.);
#2442=FACE_OUTER_BOUND('',#3539,.T.);
#2443=FACE_OUTER_BOUND('',#3540,.T.);
#2444=FACE_OUTER_BOUND('',#3541,.T.);
#2445=FACE_OUTER_BOUND('',#3542,.T.);
#2446=FACE_OUTER_BOUND('',#3543,.T.);
#2447=FACE_OUTER_BOUND('',#3544,.T.);
#2448=FACE_OUTER_BOUND('',#3545,.T.);
#2449=FACE_OUTER_BOUND('',#3546,.T.);
#2450=FACE_OUTER_BOUND('',#3547,.T.);
#2451=FACE_OUTER_BOUND('',#3548,.T.);
#2452=FACE_OUTER_BOUND('',#3549,.T.);
#2453=FACE_OUTER_BOUND('',#3550,.T.);
#2454=FACE_OUTER_BOUND('',#3551,.T.);
#2455=FACE_OUTER_BOUND('',#3552,.T.);
#2456=FACE_OUTER_BOUND('',#3553,.T.);
#2457=FACE_OUTER_BOUND('',#3554,.T.);
#2458=FACE_OUTER_BOUND('',#3555,.T.);
#2459=FACE_OUTER_BOUND('',#3556,.T.);
#2460=FACE_OUTER_BOUND('',#3557,.T.);
#2461=FACE_OUTER_BOUND('',#3558,.T.);
#2462=FACE_OUTER_BOUND('',#3559,.T.);
#2463=FACE_OUTER_BOUND('',#3560,.T.);
#2464=FACE_OUTER_BOUND('',#3561,.T.);
#2465=FACE_OUTER_BOUND('',#3562,.T.);
#2466=FACE_OUTER_BOUND('',#3563,.T.);
#2467=FACE_OUTER_BOUND('',#3564,.T.);
#2468=FACE_OUTER_BOUND('',#3565,.T.);
#2469=FACE_OUTER_BOUND('',#3566,.T.);
#2470=FACE_OUTER_BOUND('',#3567,.T.);
#2471=FACE_OUTER_BOUND('',#3568,.T.);
#2472=FACE_OUTER_BOUND('',#3569,.T.);
#2473=FACE_OUTER_BOUND('',#3570,.T.);
#2474=FACE_OUTER_BOUND('',#3571,.T.);
#2475=FACE_OUTER_BOUND('',#3572,.T.);
#2476=FACE_OUTER_BOUND('',#3573,.T.);
#2477=FACE_OUTER_BOUND('',#3574,.T.);
#2478=FACE_OUTER_BOUND('',#3575,.T.);
#2479=FACE_OUTER_BOUND('',#3576,.T.);
#2480=FACE_OUTER_BOUND('',#3577,.T.);
#2481=FACE_OUTER_BOUND('',#3578,.T.);
#2482=FACE_OUTER_BOUND('',#3579,.T.);
#2483=FACE_OUTER_BOUND('',#3580,.T.);
#2484=FACE_OUTER_BOUND('',#3581,.T.);
#2485=FACE_OUTER_BOUND('',#3582,.T.);
#2486=FACE_OUTER_BOUND('',#3583,.T.);
#2487=FACE_OUTER_BOUND('',#3584,.T.);
#2488=FACE_OUTER_BOUND('',#3585,.T.);
#2489=FACE_OUTER_BOUND('',#3586,.T.);
#2490=FACE_OUTER_BOUND('',#3587,.T.);
#2491=FACE_OUTER_BOUND('',#3588,.T.);
#2492=FACE_OUTER_BOUND('',#3589,.T.);
#2493=FACE_OUTER_BOUND('',#3590,.T.);
#2494=FACE_OUTER_BOUND('',#3591,.T.);
#2495=FACE_OUTER_BOUND('',#3592,.T.);
#2496=FACE_OUTER_BOUND('',#3593,.T.);
#2497=FACE_OUTER_BOUND('',#3594,.T.);
#2498=FACE_OUTER_BOUND('',#3595,.T.);
#2499=FACE_OUTER_BOUND('',#3596,.T.);
#2500=FACE_OUTER_BOUND('',#3597,.T.);
#2501=FACE_OUTER_BOUND('',#3598,.T.);
#2502=FACE_OUTER_BOUND('',#3599,.T.);
#2503=FACE_OUTER_BOUND('',#3600,.T.);
#2504=FACE_OUTER_BOUND('',#3601,.T.);
#2505=FACE_OUTER_BOUND('',#3602,.T.);
#2506=FACE_OUTER_BOUND('',#3603,.T.);
#2507=FACE_OUTER_BOUND('',#3604,.T.);
#2508=FACE_OUTER_BOUND('',#3605,.T.);
#2509=FACE_OUTER_BOUND('',#3606,.T.);
#2510=FACE_OUTER_BOUND('',#3607,.T.);
#2511=FACE_OUTER_BOUND('',#3608,.T.);
#2512=FACE_OUTER_BOUND('',#3609,.T.);
#2513=FACE_OUTER_BOUND('',#3610,.T.);
#2514=FACE_OUTER_BOUND('',#3611,.T.);
#2515=FACE_OUTER_BOUND('',#3612,.T.);
#2516=FACE_OUTER_BOUND('',#3613,.T.);
#2517=FACE_OUTER_BOUND('',#3614,.T.);
#2518=FACE_OUTER_BOUND('',#3615,.T.);
#2519=FACE_OUTER_BOUND('',#3616,.T.);
#2520=FACE_OUTER_BOUND('',#3617,.T.);
#2521=FACE_OUTER_BOUND('',#3618,.T.);
#2522=FACE_OUTER_BOUND('',#3619,.T.);
#2523=FACE_OUTER_BOUND('',#3621,.T.);
#2524=FACE_OUTER_BOUND('',#3622,.T.);
#2525=FACE_OUTER_BOUND('',#3623,.T.);
#2526=FACE_OUTER_BOUND('',#3624,.T.);
#2527=FACE_OUTER_BOUND('',#3625,.T.);
#2528=FACE_OUTER_BOUND('',#3626,.T.);
#2529=FACE_OUTER_BOUND('',#3627,.T.);
#2530=FACE_OUTER_BOUND('',#3628,.T.);
#2531=FACE_OUTER_BOUND('',#3629,.T.);
#2532=FACE_OUTER_BOUND('',#3630,.T.);
#2533=FACE_OUTER_BOUND('',#3631,.T.);
#2534=FACE_OUTER_BOUND('',#3632,.T.);
#2535=FACE_OUTER_BOUND('',#3633,.T.);
#2536=FACE_OUTER_BOUND('',#3634,.T.);
#2537=FACE_OUTER_BOUND('',#3635,.T.);
#2538=FACE_OUTER_BOUND('',#3636,.T.);
#2539=FACE_OUTER_BOUND('',#3637,.T.);
#2540=FACE_OUTER_BOUND('',#3638,.T.);
#2541=FACE_OUTER_BOUND('',#3639,.T.);
#2542=FACE_OUTER_BOUND('',#3640,.T.);
#2543=FACE_OUTER_BOUND('',#3641,.T.);
#2544=FACE_OUTER_BOUND('',#3642,.T.);
#2545=FACE_OUTER_BOUND('',#3643,.T.);
#2546=FACE_OUTER_BOUND('',#3645,.T.);
#2547=FACE_OUTER_BOUND('',#3647,.T.);
#2548=FACE_OUTER_BOUND('',#3648,.T.);
#2549=FACE_OUTER_BOUND('',#3649,.T.);
#2550=FACE_OUTER_BOUND('',#3650,.T.);
#2551=FACE_OUTER_BOUND('',#3651,.T.);
#2552=FACE_OUTER_BOUND('',#3652,.T.);
#2553=FACE_OUTER_BOUND('',#3653,.T.);
#2554=FACE_OUTER_BOUND('',#3654,.T.);
#2555=FACE_OUTER_BOUND('',#3655,.T.);
#2556=FACE_OUTER_BOUND('',#3656,.T.);
#2557=FACE_OUTER_BOUND('',#3657,.T.);
#2558=FACE_OUTER_BOUND('',#3659,.T.);
#2559=FACE_OUTER_BOUND('',#3661,.T.);
#2560=FACE_OUTER_BOUND('',#3662,.T.);
#2561=FACE_OUTER_BOUND('',#3663,.T.);
#2562=FACE_OUTER_BOUND('',#3664,.T.);
#2563=FACE_OUTER_BOUND('',#3665,.T.);
#2564=FACE_OUTER_BOUND('',#3666,.T.);
#2565=FACE_OUTER_BOUND('',#3667,.T.);
#2566=FACE_OUTER_BOUND('',#3668,.T.);
#2567=FACE_OUTER_BOUND('',#3669,.T.);
#2568=FACE_OUTER_BOUND('',#3670,.T.);
#2569=FACE_OUTER_BOUND('',#3671,.T.);
#2570=FACE_OUTER_BOUND('',#3672,.T.);
#2571=EDGE_LOOP('',(#9907,#9908,#9909,#9910));
#2572=EDGE_LOOP('',(#9911,#9912,#9913,#9914));
#2573=EDGE_LOOP('',(#9915,#9916,#9917,#9918));
#2574=EDGE_LOOP('',(#9919,#9920,#9921,#9922));
#2575=EDGE_LOOP('',(#9923,#9924,#9925,#9926));
#2576=EDGE_LOOP('',(#9927,#9928,#9929,#9930));
#2577=EDGE_LOOP('',(#9931,#9932,#9933,#9934));
#2578=EDGE_LOOP('',(#9935,#9936,#9937,#9938));
#2579=EDGE_LOOP('',(#9939,#9940,#9941,#9942));
#2580=EDGE_LOOP('',(#9943,#9944,#9945,#9946));
#2581=EDGE_LOOP('',(#9947,#9948,#9949,#9950));
#2582=EDGE_LOOP('',(#9951,#9952,#9953,#9954));
#2583=EDGE_LOOP('',(#9955,#9956,#9957,#9958));
#2584=EDGE_LOOP('',(#9959,#9960,#9961,#9962));
#2585=EDGE_LOOP('',(#9963,#9964,#9965,#9966));
#2586=EDGE_LOOP('',(#9967,#9968,#9969,#9970));
#2587=EDGE_LOOP('',(#9971,#9972,#9973,#9974));
#2588=EDGE_LOOP('',(#9975,#9976,#9977,#9978));
#2589=EDGE_LOOP('',(#9979,#9980,#9981,#9982,#9983,#9984));
#2590=EDGE_LOOP('',(#9985,#9986,#9987,#9988,#9989,#9990));
#2591=EDGE_LOOP('',(#9991,#9992,#9993,#9994));
#2592=EDGE_LOOP('',(#9995,#9996,#9997,#9998));
#2593=EDGE_LOOP('',(#9999,#10000,#10001,#10002));
#2594=EDGE_LOOP('',(#10003,#10004,#10005,#10006));
#2595=EDGE_LOOP('',(#10007,#10008,#10009,#10010));
#2596=EDGE_LOOP('',(#10011,#10012,#10013,#10014));
#2597=EDGE_LOOP('',(#10015,#10016,#10017,#10018,#10019,#10020));
#2598=EDGE_LOOP('',(#10021,#10022,#10023,#10024,#10025,#10026));
#2599=EDGE_LOOP('',(#10027,#10028,#10029,#10030));
#2600=EDGE_LOOP('',(#10031,#10032,#10033,#10034));
#2601=EDGE_LOOP('',(#10035,#10036,#10037,#10038));
#2602=EDGE_LOOP('',(#10039,#10040,#10041,#10042));
#2603=EDGE_LOOP('',(#10043,#10044,#10045,#10046));
#2604=EDGE_LOOP('',(#10047,#10048,#10049,#10050));
#2605=EDGE_LOOP('',(#10051,#10052,#10053,#10054));
#2606=EDGE_LOOP('',(#10055));
#2607=EDGE_LOOP('',(#10056));
#2608=EDGE_LOOP('',(#10057));
#2609=EDGE_LOOP('',(#10058));
#2610=EDGE_LOOP('',(#10059));
#2611=EDGE_LOOP('',(#10060));
#2612=EDGE_LOOP('',(#10061,#10062,#10063,#10064));
#2613=EDGE_LOOP('',(#10065));
#2614=EDGE_LOOP('',(#10066));
#2615=EDGE_LOOP('',(#10067));
#2616=EDGE_LOOP('',(#10068));
#2617=EDGE_LOOP('',(#10069));
#2618=EDGE_LOOP('',(#10070));
#2619=EDGE_LOOP('',(#10071,#10072,#10073,#10074));
#2620=EDGE_LOOP('',(#10075,#10076,#10077,#10078));
#2621=EDGE_LOOP('',(#10079,#10080,#10081,#10082));
#2622=EDGE_LOOP('',(#10083,#10084,#10085,#10086));
#2623=EDGE_LOOP('',(#10087,#10088,#10089,#10090));
#2624=EDGE_LOOP('',(#10091,#10092,#10093,#10094));
#2625=EDGE_LOOP('',(#10095,#10096,#10097,#10098));
#2626=EDGE_LOOP('',(#10099,#10100,#10101,#10102));
#2627=EDGE_LOOP('',(#10103,#10104,#10105,#10106));
#2628=EDGE_LOOP('',(#10107,#10108,#10109,#10110));
#2629=EDGE_LOOP('',(#10111,#10112,#10113,#10114));
#2630=EDGE_LOOP('',(#10115,#10116,#10117,#10118));
#2631=EDGE_LOOP('',(#10119,#10120,#10121,#10122));
#2632=EDGE_LOOP('',(#10123,#10124,#10125,#10126));
#2633=EDGE_LOOP('',(#10127));
#2634=EDGE_LOOP('',(#10128));
#2635=EDGE_LOOP('',(#10129));
#2636=EDGE_LOOP('',(#10130));
#2637=EDGE_LOOP('',(#10131));
#2638=EDGE_LOOP('',(#10132,#10133,#10134,#10135));
#2639=EDGE_LOOP('',(#10136));
#2640=EDGE_LOOP('',(#10137));
#2641=EDGE_LOOP('',(#10138));
#2642=EDGE_LOOP('',(#10139));
#2643=EDGE_LOOP('',(#10140));
#2644=EDGE_LOOP('',(#10141,#10142,#10143,#10144));
#2645=EDGE_LOOP('',(#10145,#10146,#10147,#10148));
#2646=EDGE_LOOP('',(#10149,#10150,#10151,#10152));
#2647=EDGE_LOOP('',(#10153,#10154,#10155,#10156));
#2648=EDGE_LOOP('',(#10157,#10158,#10159,#10160));
#2649=EDGE_LOOP('',(#10161,#10162,#10163,#10164));
#2650=EDGE_LOOP('',(#10165,#10166,#10167,#10168));
#2651=EDGE_LOOP('',(#10169,#10170,#10171,#10172));
#2652=EDGE_LOOP('',(#10173,#10174,#10175,#10176));
#2653=EDGE_LOOP('',(#10177,#10178,#10179,#10180));
#2654=EDGE_LOOP('',(#10181));
#2655=EDGE_LOOP('',(#10182));
#2656=EDGE_LOOP('',(#10183));
#2657=EDGE_LOOP('',(#10184));
#2658=EDGE_LOOP('',(#10185));
#2659=EDGE_LOOP('',(#10186,#10187,#10188,#10189));
#2660=EDGE_LOOP('',(#10190));
#2661=EDGE_LOOP('',(#10191));
#2662=EDGE_LOOP('',(#10192));
#2663=EDGE_LOOP('',(#10193));
#2664=EDGE_LOOP('',(#10194));
#2665=EDGE_LOOP('',(#10195,#10196,#10197,#10198));
#2666=EDGE_LOOP('',(#10199,#10200,#10201,#10202));
#2667=EDGE_LOOP('',(#10203,#10204,#10205,#10206));
#2668=EDGE_LOOP('',(#10207,#10208,#10209,#10210));
#2669=EDGE_LOOP('',(#10211,#10212,#10213,#10214));
#2670=EDGE_LOOP('',(#10215,#10216,#10217,#10218));
#2671=EDGE_LOOP('',(#10219,#10220,#10221,#10222));
#2672=EDGE_LOOP('',(#10223,#10224,#10225,#10226));
#2673=EDGE_LOOP('',(#10227,#10228,#10229,#10230));
#2674=EDGE_LOOP('',(#10231,#10232,#10233,#10234));
#2675=EDGE_LOOP('',(#10235,#10236,#10237,#10238));
#2676=EDGE_LOOP('',(#10239,#10240,#10241,#10242));
#2677=EDGE_LOOP('',(#10243,#10244,#10245,#10246));
#2678=EDGE_LOOP('',(#10247,#10248,#10249,#10250));
#2679=EDGE_LOOP('',(#10251,#10252,#10253,#10254));
#2680=EDGE_LOOP('',(#10255,#10256,#10257,#10258));
#2681=EDGE_LOOP('',(#10259,#10260,#10261,#10262));
#2682=EDGE_LOOP('',(#10263,#10264,#10265,#10266));
#2683=EDGE_LOOP('',(#10267,#10268,#10269,#10270));
#2684=EDGE_LOOP('',(#10271,#10272,#10273,#10274));
#2685=EDGE_LOOP('',(#10275,#10276,#10277,#10278));
#2686=EDGE_LOOP('',(#10279,#10280,#10281,#10282));
#2687=EDGE_LOOP('',(#10283,#10284,#10285,#10286));
#2688=EDGE_LOOP('',(#10287,#10288,#10289,#10290));
#2689=EDGE_LOOP('',(#10291,#10292,#10293,#10294));
#2690=EDGE_LOOP('',(#10295,#10296,#10297,#10298));
#2691=EDGE_LOOP('',(#10299,#10300,#10301,#10302));
#2692=EDGE_LOOP('',(#10303,#10304,#10305,#10306));
#2693=EDGE_LOOP('',(#10307,#10308,#10309,#10310));
#2694=EDGE_LOOP('',(#10311,#10312,#10313,#10314));
#2695=EDGE_LOOP('',(#10315,#10316,#10317,#10318));
#2696=EDGE_LOOP('',(#10319,#10320,#10321,#10322));
#2697=EDGE_LOOP('',(#10323,#10324,#10325,#10326));
#2698=EDGE_LOOP('',(#10327,#10328,#10329,#10330));
#2699=EDGE_LOOP('',(#10331,#10332,#10333,#10334));
#2700=EDGE_LOOP('',(#10335,#10336,#10337,#10338));
#2701=EDGE_LOOP('',(#10339,#10340,#10341,#10342));
#2702=EDGE_LOOP('',(#10343,#10344,#10345,#10346));
#2703=EDGE_LOOP('',(#10347,#10348,#10349,#10350));
#2704=EDGE_LOOP('',(#10351,#10352,#10353,#10354));
#2705=EDGE_LOOP('',(#10355,#10356,#10357,#10358));
#2706=EDGE_LOOP('',(#10359));
#2707=EDGE_LOOP('',(#10360));
#2708=EDGE_LOOP('',(#10361));
#2709=EDGE_LOOP('',(#10362));
#2710=EDGE_LOOP('',(#10363));
#2711=EDGE_LOOP('',(#10364));
#2712=EDGE_LOOP('',(#10365));
#2713=EDGE_LOOP('',(#10366));
#2714=EDGE_LOOP('',(#10367));
#2715=EDGE_LOOP('',(#10368));
#2716=EDGE_LOOP('',(#10369));
#2717=EDGE_LOOP('',(#10370));
#2718=EDGE_LOOP('',(#10371));
#2719=EDGE_LOOP('',(#10372));
#2720=EDGE_LOOP('',(#10373));
#2721=EDGE_LOOP('',(#10374));
#2722=EDGE_LOOP('',(#10375));
#2723=EDGE_LOOP('',(#10376));
#2724=EDGE_LOOP('',(#10377,#10378,#10379,#10380));
#2725=EDGE_LOOP('',(#10381));
#2726=EDGE_LOOP('',(#10382));
#2727=EDGE_LOOP('',(#10383));
#2728=EDGE_LOOP('',(#10384));
#2729=EDGE_LOOP('',(#10385));
#2730=EDGE_LOOP('',(#10386));
#2731=EDGE_LOOP('',(#10387));
#2732=EDGE_LOOP('',(#10388));
#2733=EDGE_LOOP('',(#10389));
#2734=EDGE_LOOP('',(#10390));
#2735=EDGE_LOOP('',(#10391));
#2736=EDGE_LOOP('',(#10392));
#2737=EDGE_LOOP('',(#10393));
#2738=EDGE_LOOP('',(#10394));
#2739=EDGE_LOOP('',(#10395));
#2740=EDGE_LOOP('',(#10396));
#2741=EDGE_LOOP('',(#10397));
#2742=EDGE_LOOP('',(#10398));
#2743=EDGE_LOOP('',(#10399,#10400,#10401,#10402));
#2744=EDGE_LOOP('',(#10403,#10404,#10405,#10406));
#2745=EDGE_LOOP('',(#10407));
#2746=EDGE_LOOP('',(#10408));
#2747=EDGE_LOOP('',(#10409));
#2748=EDGE_LOOP('',(#10410));
#2749=EDGE_LOOP('',(#10411,#10412,#10413,#10414));
#2750=EDGE_LOOP('',(#10415,#10416,#10417,#10418));
#2751=EDGE_LOOP('',(#10419));
#2752=EDGE_LOOP('',(#10420));
#2753=EDGE_LOOP('',(#10421));
#2754=EDGE_LOOP('',(#10422));
#2755=EDGE_LOOP('',(#10423,#10424,#10425,#10426));
#2756=EDGE_LOOP('',(#10427,#10428,#10429,#10430));
#2757=EDGE_LOOP('',(#10431,#10432,#10433,#10434));
#2758=EDGE_LOOP('',(#10435,#10436,#10437,#10438));
#2759=EDGE_LOOP('',(#10439,#10440,#10441,#10442));
#2760=EDGE_LOOP('',(#10443,#10444,#10445,#10446));
#2761=EDGE_LOOP('',(#10447,#10448,#10449,#10450));
#2762=EDGE_LOOP('',(#10451,#10452,#10453,#10454));
#2763=EDGE_LOOP('',(#10455,#10456,#10457,#10458));
#2764=EDGE_LOOP('',(#10459,#10460,#10461,#10462));
#2765=EDGE_LOOP('',(#10463,#10464,#10465,#10466));
#2766=EDGE_LOOP('',(#10467,#10468,#10469,#10470));
#2767=EDGE_LOOP('',(#10471,#10472,#10473,#10474));
#2768=EDGE_LOOP('',(#10475,#10476,#10477,#10478));
#2769=EDGE_LOOP('',(#10479));
#2770=EDGE_LOOP('',(#10480));
#2771=EDGE_LOOP('',(#10481));
#2772=EDGE_LOOP('',(#10482));
#2773=EDGE_LOOP('',(#10483));
#2774=EDGE_LOOP('',(#10484));
#2775=EDGE_LOOP('',(#10485));
#2776=EDGE_LOOP('',(#10486));
#2777=EDGE_LOOP('',(#10487));
#2778=EDGE_LOOP('',(#10488));
#2779=EDGE_LOOP('',(#10489));
#2780=EDGE_LOOP('',(#10490));
#2781=EDGE_LOOP('',(#10491));
#2782=EDGE_LOOP('',(#10492));
#2783=EDGE_LOOP('',(#10493));
#2784=EDGE_LOOP('',(#10494));
#2785=EDGE_LOOP('',(#10495));
#2786=EDGE_LOOP('',(#10496));
#2787=EDGE_LOOP('',(#10497));
#2788=EDGE_LOOP('',(#10498));
#2789=EDGE_LOOP('',(#10499));
#2790=EDGE_LOOP('',(#10500));
#2791=EDGE_LOOP('',(#10501));
#2792=EDGE_LOOP('',(#10502));
#2793=EDGE_LOOP('',(#10503));
#2794=EDGE_LOOP('',(#10504));
#2795=EDGE_LOOP('',(#10505));
#2796=EDGE_LOOP('',(#10506));
#2797=EDGE_LOOP('',(#10507,#10508,#10509,#10510));
#2798=EDGE_LOOP('',(#10511,#10512,#10513,#10514));
#2799=EDGE_LOOP('',(#10515,#10516,#10517,#10518));
#2800=EDGE_LOOP('',(#10519,#10520,#10521,#10522));
#2801=EDGE_LOOP('',(#10523,#10524,#10525,#10526));
#2802=EDGE_LOOP('',(#10527,#10528,#10529,#10530));
#2803=EDGE_LOOP('',(#10531));
#2804=EDGE_LOOP('',(#10532));
#2805=EDGE_LOOP('',(#10533));
#2806=EDGE_LOOP('',(#10534));
#2807=EDGE_LOOP('',(#10535));
#2808=EDGE_LOOP('',(#10536));
#2809=EDGE_LOOP('',(#10537));
#2810=EDGE_LOOP('',(#10538));
#2811=EDGE_LOOP('',(#10539));
#2812=EDGE_LOOP('',(#10540));
#2813=EDGE_LOOP('',(#10541));
#2814=EDGE_LOOP('',(#10542));
#2815=EDGE_LOOP('',(#10543,#10544,#10545,#10546,#10547,#10548,#10549,#10550,
#10551));
#2816=EDGE_LOOP('',(#10552,#10553,#10554,#10555,#10556,#10557,#10558,#10559,
#10560));
#2817=EDGE_LOOP('',(#10561,#10562,#10563,#10564));
#2818=EDGE_LOOP('',(#10565,#10566,#10567,#10568));
#2819=EDGE_LOOP('',(#10569,#10570,#10571,#10572));
#2820=EDGE_LOOP('',(#10573,#10574,#10575,#10576));
#2821=EDGE_LOOP('',(#10577,#10578,#10579,#10580));
#2822=EDGE_LOOP('',(#10581,#10582,#10583,#10584));
#2823=EDGE_LOOP('',(#10585,#10586,#10587,#10588));
#2824=EDGE_LOOP('',(#10589,#10590,#10591,#10592));
#2825=EDGE_LOOP('',(#10593,#10594,#10595,#10596));
#2826=EDGE_LOOP('',(#10597,#10598,#10599,#10600,#10601,#10602,#10603,#10604,
#10605));
#2827=EDGE_LOOP('',(#10606,#10607,#10608,#10609,#10610,#10611,#10612,#10613,
#10614));
#2828=EDGE_LOOP('',(#10615,#10616,#10617,#10618));
#2829=EDGE_LOOP('',(#10619,#10620,#10621,#10622));
#2830=EDGE_LOOP('',(#10623,#10624,#10625,#10626));
#2831=EDGE_LOOP('',(#10627,#10628,#10629,#10630));
#2832=EDGE_LOOP('',(#10631,#10632,#10633,#10634));
#2833=EDGE_LOOP('',(#10635,#10636,#10637,#10638));
#2834=EDGE_LOOP('',(#10639,#10640,#10641,#10642));
#2835=EDGE_LOOP('',(#10643,#10644,#10645,#10646));
#2836=EDGE_LOOP('',(#10647,#10648,#10649,#10650));
#2837=EDGE_LOOP('',(#10651,#10652,#10653,#10654,#10655,#10656,#10657,#10658,
#10659));
#2838=EDGE_LOOP('',(#10660,#10661,#10662,#10663,#10664,#10665,#10666,#10667,
#10668));
#2839=EDGE_LOOP('',(#10669,#10670,#10671,#10672));
#2840=EDGE_LOOP('',(#10673,#10674,#10675,#10676));
#2841=EDGE_LOOP('',(#10677,#10678,#10679,#10680));
#2842=EDGE_LOOP('',(#10681,#10682,#10683,#10684));
#2843=EDGE_LOOP('',(#10685,#10686,#10687,#10688));
#2844=EDGE_LOOP('',(#10689,#10690,#10691,#10692));
#2845=EDGE_LOOP('',(#10693,#10694,#10695,#10696));
#2846=EDGE_LOOP('',(#10697,#10698,#10699,#10700));
#2847=EDGE_LOOP('',(#10701,#10702,#10703,#10704));
#2848=EDGE_LOOP('',(#10705,#10706,#10707,#10708));
#2849=EDGE_LOOP('',(#10709,#10710,#10711,#10712));
#2850=EDGE_LOOP('',(#10713,#10714,#10715,#10716));
#2851=EDGE_LOOP('',(#10717,#10718,#10719,#10720));
#2852=EDGE_LOOP('',(#10721,#10722,#10723,#10724));
#2853=EDGE_LOOP('',(#10725,#10726,#10727,#10728));
#2854=EDGE_LOOP('',(#10729,#10730,#10731,#10732));
#2855=EDGE_LOOP('',(#10733,#10734,#10735,#10736,#10737,#10738));
#2856=EDGE_LOOP('',(#10739));
#2857=EDGE_LOOP('',(#10740,#10741,#10742,#10743,#10744,#10745));
#2858=EDGE_LOOP('',(#10746));
#2859=EDGE_LOOP('',(#10747,#10748,#10749,#10750));
#2860=EDGE_LOOP('',(#10751,#10752,#10753,#10754,#10755,#10756));
#2861=EDGE_LOOP('',(#10757));
#2862=EDGE_LOOP('',(#10758,#10759,#10760,#10761,#10762,#10763));
#2863=EDGE_LOOP('',(#10764));
#2864=EDGE_LOOP('',(#10765,#10766,#10767,#10768));
#2865=EDGE_LOOP('',(#10769,#10770,#10771,#10772));
#2866=EDGE_LOOP('',(#10773,#10774,#10775,#10776));
#2867=EDGE_LOOP('',(#10777,#10778,#10779,#10780));
#2868=EDGE_LOOP('',(#10781,#10782,#10783,#10784));
#2869=EDGE_LOOP('',(#10785,#10786,#10787,#10788));
#2870=EDGE_LOOP('',(#10789,#10790,#10791,#10792));
#2871=EDGE_LOOP('',(#10793,#10794,#10795,#10796));
#2872=EDGE_LOOP('',(#10797,#10798,#10799,#10800));
#2873=EDGE_LOOP('',(#10801,#10802,#10803,#10804));
#2874=EDGE_LOOP('',(#10805,#10806,#10807,#10808));
#2875=EDGE_LOOP('',(#10809,#10810,#10811,#10812));
#2876=EDGE_LOOP('',(#10813,#10814,#10815,#10816));
#2877=EDGE_LOOP('',(#10817,#10818,#10819,#10820,#10821,#10822));
#2878=EDGE_LOOP('',(#10823));
#2879=EDGE_LOOP('',(#10824,#10825,#10826,#10827,#10828,#10829));
#2880=EDGE_LOOP('',(#10830));
#2881=EDGE_LOOP('',(#10831,#10832,#10833,#10834));
#2882=EDGE_LOOP('',(#10835,#10836,#10837,#10838,#10839,#10840));
#2883=EDGE_LOOP('',(#10841));
#2884=EDGE_LOOP('',(#10842,#10843,#10844,#10845,#10846,#10847));
#2885=EDGE_LOOP('',(#10848));
#2886=EDGE_LOOP('',(#10849,#10850,#10851,#10852));
#2887=EDGE_LOOP('',(#10853,#10854,#10855,#10856));
#2888=EDGE_LOOP('',(#10857,#10858,#10859,#10860));
#2889=EDGE_LOOP('',(#10861,#10862,#10863,#10864));
#2890=EDGE_LOOP('',(#10865,#10866,#10867,#10868));
#2891=EDGE_LOOP('',(#10869,#10870,#10871,#10872));
#2892=EDGE_LOOP('',(#10873,#10874,#10875,#10876));
#2893=EDGE_LOOP('',(#10877,#10878,#10879,#10880));
#2894=EDGE_LOOP('',(#10881,#10882,#10883,#10884));
#2895=EDGE_LOOP('',(#10885,#10886,#10887,#10888));
#2896=EDGE_LOOP('',(#10889,#10890,#10891,#10892));
#2897=EDGE_LOOP('',(#10893,#10894,#10895,#10896));
#2898=EDGE_LOOP('',(#10897,#10898,#10899,#10900,#10901,#10902,#10903,#10904,
#10905));
#2899=EDGE_LOOP('',(#10906,#10907,#10908,#10909,#10910,#10911,#10912,#10913,
#10914));
#2900=EDGE_LOOP('',(#10915,#10916,#10917,#10918,#10919,#10920,#10921,#10922,
#10923,#10924,#10925,#10926));
#2901=EDGE_LOOP('',(#10927,#10928,#10929,#10930));
#2902=EDGE_LOOP('',(#10931,#10932,#10933,#10934));
#2903=EDGE_LOOP('',(#10935,#10936,#10937,#10938));
#2904=EDGE_LOOP('',(#10939,#10940,#10941,#10942));
#2905=EDGE_LOOP('',(#10943,#10944,#10945,#10946));
#2906=EDGE_LOOP('',(#10947,#10948,#10949,#10950,#10951,#10952,#10953,#10954,
#10955,#10956,#10957,#10958));
#2907=EDGE_LOOP('',(#10959,#10960,#10961,#10962));
#2908=EDGE_LOOP('',(#10963,#10964,#10965,#10966));
#2909=EDGE_LOOP('',(#10967,#10968,#10969,#10970,#10971));
#2910=EDGE_LOOP('',(#10972,#10973,#10974,#10975,#10976));
#2911=EDGE_LOOP('',(#10977,#10978,#10979,#10980,#10981));
#2912=EDGE_LOOP('',(#10982,#10983,#10984,#10985,#10986));
#2913=EDGE_LOOP('',(#10987,#10988,#10989,#10990));
#2914=EDGE_LOOP('',(#10991,#10992,#10993,#10994,#10995,#10996));
#2915=EDGE_LOOP('',(#10997));
#2916=EDGE_LOOP('',(#10998,#10999,#11000,#11001,#11002,#11003));
#2917=EDGE_LOOP('',(#11004));
#2918=EDGE_LOOP('',(#11005,#11006,#11007,#11008));
#2919=EDGE_LOOP('',(#11009,#11010,#11011,#11012));
#2920=EDGE_LOOP('',(#11013,#11014,#11015,#11016));
#2921=EDGE_LOOP('',(#11017,#11018,#11019,#11020));
#2922=EDGE_LOOP('',(#11021,#11022,#11023,#11024));
#2923=EDGE_LOOP('',(#11025,#11026,#11027,#11028));
#2924=EDGE_LOOP('',(#11029,#11030,#11031,#11032));
#2925=EDGE_LOOP('',(#11033,#11034,#11035,#11036,#11037,#11038));
#2926=EDGE_LOOP('',(#11039));
#2927=EDGE_LOOP('',(#11040,#11041,#11042,#11043,#11044,#11045));
#2928=EDGE_LOOP('',(#11046));
#2929=EDGE_LOOP('',(#11047,#11048,#11049,#11050));
#2930=EDGE_LOOP('',(#11051,#11052,#11053,#11054));
#2931=EDGE_LOOP('',(#11055,#11056,#11057,#11058));
#2932=EDGE_LOOP('',(#11059,#11060,#11061,#11062));
#2933=EDGE_LOOP('',(#11063,#11064,#11065,#11066));
#2934=EDGE_LOOP('',(#11067,#11068,#11069,#11070));
#2935=EDGE_LOOP('',(#11071,#11072,#11073,#11074));
#2936=EDGE_LOOP('',(#11075,#11076,#11077,#11078));
#2937=EDGE_LOOP('',(#11079,#11080,#11081,#11082));
#2938=EDGE_LOOP('',(#11083,#11084,#11085,#11086));
#2939=EDGE_LOOP('',(#11087,#11088,#11089,#11090));
#2940=EDGE_LOOP('',(#11091,#11092,#11093,#11094));
#2941=EDGE_LOOP('',(#11095,#11096,#11097,#11098));
#2942=EDGE_LOOP('',(#11099,#11100,#11101,#11102));
#2943=EDGE_LOOP('',(#11103,#11104,#11105,#11106));
#2944=EDGE_LOOP('',(#11107,#11108,#11109,#11110));
#2945=EDGE_LOOP('',(#11111,#11112,#11113,#11114));
#2946=EDGE_LOOP('',(#11115,#11116,#11117,#11118));
#2947=EDGE_LOOP('',(#11119,#11120,#11121,#11122,#11123,#11124,#11125,#11126,
#11127,#11128,#11129,#11130));
#2948=EDGE_LOOP('',(#11131,#11132,#11133,#11134,#11135,#11136,#11137,#11138,
#11139,#11140,#11141,#11142));
#2949=EDGE_LOOP('',(#11143,#11144,#11145,#11146));
#2950=EDGE_LOOP('',(#11147,#11148,#11149,#11150));
#2951=EDGE_LOOP('',(#11151,#11152,#11153,#11154));
#2952=EDGE_LOOP('',(#11155,#11156,#11157,#11158,#11159,#11160));
#2953=EDGE_LOOP('',(#11161));
#2954=EDGE_LOOP('',(#11162,#11163,#11164,#11165,#11166,#11167));
#2955=EDGE_LOOP('',(#11168));
#2956=EDGE_LOOP('',(#11169,#11170,#11171,#11172));
#2957=EDGE_LOOP('',(#11173,#11174,#11175,#11176));
#2958=EDGE_LOOP('',(#11177,#11178,#11179,#11180));
#2959=EDGE_LOOP('',(#11181,#11182,#11183,#11184));
#2960=EDGE_LOOP('',(#11185,#11186,#11187,#11188));
#2961=EDGE_LOOP('',(#11189,#11190,#11191,#11192));
#2962=EDGE_LOOP('',(#11193,#11194,#11195,#11196));
#2963=EDGE_LOOP('',(#11197,#11198,#11199,#11200,#11201,#11202));
#2964=EDGE_LOOP('',(#11203));
#2965=EDGE_LOOP('',(#11204,#11205,#11206,#11207,#11208,#11209));
#2966=EDGE_LOOP('',(#11210));
#2967=EDGE_LOOP('',(#11211,#11212,#11213,#11214));
#2968=EDGE_LOOP('',(#11215,#11216,#11217,#11218));
#2969=EDGE_LOOP('',(#11219,#11220,#11221,#11222));
#2970=EDGE_LOOP('',(#11223,#11224,#11225,#11226));
#2971=EDGE_LOOP('',(#11227,#11228,#11229,#11230,#11231));
#2972=EDGE_LOOP('',(#11232,#11233,#11234,#11235,#11236));
#2973=EDGE_LOOP('',(#11237,#11238,#11239,#11240));
#2974=EDGE_LOOP('',(#11241,#11242,#11243,#11244,#11245,#11246));
#2975=EDGE_LOOP('',(#11247,#11248,#11249,#11250));
#2976=EDGE_LOOP('',(#11251));
#2977=EDGE_LOOP('',(#11252));
#2978=EDGE_LOOP('',(#11253,#11254,#11255,#11256));
#2979=EDGE_LOOP('',(#11257,#11258,#11259,#11260));
#2980=EDGE_LOOP('',(#11261,#11262,#11263,#11264,#11265));
#2981=EDGE_LOOP('',(#11266,#11267,#11268,#11269,#11270));
#2982=EDGE_LOOP('',(#11271,#11272,#11273,#11274,#11275));
#2983=EDGE_LOOP('',(#11276,#11277,#11278,#11279,#11280));
#2984=EDGE_LOOP('',(#11281,#11282,#11283,#11284,#11285));
#2985=EDGE_LOOP('',(#11286,#11287,#11288,#11289,#11290));
#2986=EDGE_LOOP('',(#11291,#11292,#11293,#11294,#11295,#11296));
#2987=EDGE_LOOP('',(#11297));
#2988=EDGE_LOOP('',(#11298));
#2989=EDGE_LOOP('',(#11299,#11300,#11301));
#2990=EDGE_LOOP('',(#11302,#11303,#11304));
#2991=EDGE_LOOP('',(#11305,#11306,#11307));
#2992=EDGE_LOOP('',(#11308,#11309,#11310));
#2993=EDGE_LOOP('',(#11311,#11312,#11313));
#2994=EDGE_LOOP('',(#11314,#11315,#11316));
#2995=EDGE_LOOP('',(#11317,#11318,#11319,#11320,#11321,#11322));
#2996=EDGE_LOOP('',(#11323,#11324,#11325,#11326));
#2997=EDGE_LOOP('',(#11327,#11328,#11329,#11330));
#2998=EDGE_LOOP('',(#11331,#11332,#11333,#11334,#11335));
#2999=EDGE_LOOP('',(#11336,#11337,#11338,#11339,#11340));
#3000=EDGE_LOOP('',(#11341,#11342,#11343,#11344,#11345));
#3001=EDGE_LOOP('',(#11346,#11347,#11348,#11349,#11350));
#3002=EDGE_LOOP('',(#11351,#11352,#11353,#11354,#11355));
#3003=EDGE_LOOP('',(#11356,#11357,#11358,#11359,#11360));
#3004=EDGE_LOOP('',(#11361,#11362,#11363,#11364,#11365,#11366));
#3005=EDGE_LOOP('',(#11367));
#3006=EDGE_LOOP('',(#11368));
#3007=EDGE_LOOP('',(#11369,#11370,#11371));
#3008=EDGE_LOOP('',(#11372,#11373,#11374));
#3009=EDGE_LOOP('',(#11375,#11376,#11377));
#3010=EDGE_LOOP('',(#11378,#11379,#11380));
#3011=EDGE_LOOP('',(#11381,#11382,#11383));
#3012=EDGE_LOOP('',(#11384,#11385,#11386));
#3013=EDGE_LOOP('',(#11387,#11388,#11389,#11390,#11391,#11392));
#3014=EDGE_LOOP('',(#11393,#11394,#11395,#11396,#11397));
#3015=EDGE_LOOP('',(#11398,#11399,#11400,#11401,#11402,#11403));
#3016=EDGE_LOOP('',(#11404,#11405,#11406,#11407));
#3017=EDGE_LOOP('',(#11408,#11409,#11410,#11411,#11412));
#3018=EDGE_LOOP('',(#11413,#11414,#11415,#11416,#11417,#11418));
#3019=EDGE_LOOP('',(#11419,#11420,#11421,#11422,#11423,#11424));
#3020=EDGE_LOOP('',(#11425,#11426,#11427,#11428,#11429,#11430));
#3021=EDGE_LOOP('',(#11431,#11432,#11433,#11434,#11435,#11436));
#3022=EDGE_LOOP('',(#11437,#11438,#11439,#11440,#11441,#11442));
#3023=EDGE_LOOP('',(#11443,#11444,#11445,#11446,#11447,#11448));
#3024=EDGE_LOOP('',(#11449,#11450,#11451,#11452,#11453,#11454));
#3025=EDGE_LOOP('',(#11455));
#3026=EDGE_LOOP('',(#11456,#11457,#11458,#11459,#11460,#11461));
#3027=EDGE_LOOP('',(#11462));
#3028=EDGE_LOOP('',(#11463,#11464,#11465));
#3029=EDGE_LOOP('',(#11466,#11467,#11468));
#3030=EDGE_LOOP('',(#11469,#11470,#11471));
#3031=EDGE_LOOP('',(#11472,#11473,#11474));
#3032=EDGE_LOOP('',(#11475,#11476,#11477));
#3033=EDGE_LOOP('',(#11478,#11479,#11480));
#3034=EDGE_LOOP('',(#11481,#11482,#11483));
#3035=EDGE_LOOP('',(#11484,#11485,#11486));
#3036=EDGE_LOOP('',(#11487,#11488,#11489));
#3037=EDGE_LOOP('',(#11490,#11491,#11492));
#3038=EDGE_LOOP('',(#11493,#11494,#11495));
#3039=EDGE_LOOP('',(#11496,#11497,#11498));
#3040=EDGE_LOOP('',(#11499,#11500,#11501,#11502));
#3041=EDGE_LOOP('',(#11503,#11504,#11505,#11506));
#3042=EDGE_LOOP('',(#11507,#11508,#11509,#11510));
#3043=EDGE_LOOP('',(#11511,#11512,#11513,#11514));
#3044=EDGE_LOOP('',(#11515,#11516,#11517,#11518));
#3045=EDGE_LOOP('',(#11519,#11520,#11521,#11522));
#3046=EDGE_LOOP('',(#11523,#11524,#11525,#11526));
#3047=EDGE_LOOP('',(#11527,#11528,#11529,#11530));
#3048=EDGE_LOOP('',(#11531,#11532,#11533,#11534));
#3049=EDGE_LOOP('',(#11535,#11536,#11537,#11538));
#3050=EDGE_LOOP('',(#11539,#11540,#11541,#11542));
#3051=EDGE_LOOP('',(#11543,#11544,#11545,#11546));
#3052=EDGE_LOOP('',(#11547,#11548,#11549,#11550));
#3053=EDGE_LOOP('',(#11551,#11552,#11553,#11554));
#3054=EDGE_LOOP('',(#11555,#11556,#11557,#11558));
#3055=EDGE_LOOP('',(#11559,#11560,#11561,#11562));
#3056=EDGE_LOOP('',(#11563,#11564,#11565,#11566));
#3057=EDGE_LOOP('',(#11567,#11568,#11569,#11570));
#3058=EDGE_LOOP('',(#11571,#11572,#11573,#11574));
#3059=EDGE_LOOP('',(#11575,#11576,#11577,#11578));
#3060=EDGE_LOOP('',(#11579,#11580,#11581,#11582));
#3061=EDGE_LOOP('',(#11583,#11584,#11585,#11586));
#3062=EDGE_LOOP('',(#11587,#11588,#11589,#11590,#11591,#11592,#11593,#11594,
#11595,#11596,#11597,#11598,#11599));
#3063=EDGE_LOOP('',(#11600,#11601,#11602,#11603));
#3064=EDGE_LOOP('',(#11604,#11605,#11606,#11607));
#3065=EDGE_LOOP('',(#11608,#11609,#11610,#11611));
#3066=EDGE_LOOP('',(#11612,#11613,#11614,#11615));
#3067=EDGE_LOOP('',(#11616,#11617,#11618,#11619));
#3068=EDGE_LOOP('',(#11620,#11621,#11622,#11623));
#3069=EDGE_LOOP('',(#11624,#11625,#11626,#11627));
#3070=EDGE_LOOP('',(#11628,#11629,#11630,#11631));
#3071=EDGE_LOOP('',(#11632,#11633,#11634,#11635));
#3072=EDGE_LOOP('',(#11636,#11637,#11638,#11639));
#3073=EDGE_LOOP('',(#11640,#11641,#11642,#11643));
#3074=EDGE_LOOP('',(#11644,#11645,#11646,#11647));
#3075=EDGE_LOOP('',(#11648,#11649,#11650,#11651));
#3076=EDGE_LOOP('',(#11652,#11653,#11654,#11655));
#3077=EDGE_LOOP('',(#11656,#11657,#11658,#11659));
#3078=EDGE_LOOP('',(#11660,#11661,#11662,#11663));
#3079=EDGE_LOOP('',(#11664,#11665,#11666,#11667));
#3080=EDGE_LOOP('',(#11668,#11669,#11670,#11671));
#3081=EDGE_LOOP('',(#11672,#11673,#11674,#11675));
#3082=EDGE_LOOP('',(#11676,#11677,#11678,#11679,#11680));
#3083=EDGE_LOOP('',(#11681,#11682,#11683,#11684));
#3084=EDGE_LOOP('',(#11685,#11686,#11687,#11688));
#3085=EDGE_LOOP('',(#11689,#11690,#11691,#11692));
#3086=EDGE_LOOP('',(#11693,#11694,#11695,#11696));
#3087=EDGE_LOOP('',(#11697,#11698,#11699,#11700,#11701,#11702,#11703,#11704,
#11705));
#3088=EDGE_LOOP('',(#11706,#11707,#11708));
#3089=EDGE_LOOP('',(#11709,#11710,#11711,#11712,#11713));
#3090=EDGE_LOOP('',(#11714));
#3091=EDGE_LOOP('',(#11715,#11716,#11717,#11718,#11719));
#3092=EDGE_LOOP('',(#11720));
#3093=EDGE_LOOP('',(#11721));
#3094=EDGE_LOOP('',(#11722,#11723,#11724,#11725));
#3095=EDGE_LOOP('',(#11726,#11727,#11728,#11729,#11730,#11731,#11732,#11733,
#11734,#11735,#11736,#11737,#11738,#11739,#11740,#11741,#11742,#11743,#11744,
#11745,#11746,#11747,#11748,#11749,#11750,#11751,#11752,#11753,#11754,#11755,
#11756,#11757,#11758,#11759,#11760,#11761,#11762,#11763,#11764,#11765,#11766,
#11767,#11768,#11769,#11770,#11771,#11772,#11773));
#3096=EDGE_LOOP('',(#11774,#11775,#11776,#11777));
#3097=EDGE_LOOP('',(#11778,#11779,#11780,#11781,#11782,#11783,#11784,#11785,
#11786,#11787,#11788,#11789,#11790,#11791,#11792,#11793,#11794,#11795,#11796,
#11797,#11798,#11799,#11800,#11801,#11802,#11803,#11804,#11805,#11806,#11807,
#11808,#11809,#11810,#11811,#11812,#11813,#11814,#11815,#11816,#11817,#11818,
#11819,#11820,#11821,#11822,#11823,#11824));
#3098=EDGE_LOOP('',(#11825,#11826,#11827));
#3099=EDGE_LOOP('',(#11828,#11829,#11830,#11831,#11832,#11833));
#3100=EDGE_LOOP('',(#11834,#11835,#11836));
#3101=EDGE_LOOP('',(#11837,#11838,#11839));
#3102=EDGE_LOOP('',(#11840,#11841,#11842,#11843,#11844,#11845));
#3103=EDGE_LOOP('',(#11846,#11847,#11848));
#3104=EDGE_LOOP('',(#11849,#11850,#11851));
#3105=EDGE_LOOP('',(#11852,#11853,#11854,#11855));
#3106=EDGE_LOOP('',(#11856,#11857,#11858,#11859));
#3107=EDGE_LOOP('',(#11860,#11861,#11862));
#3108=EDGE_LOOP('',(#11863,#11864,#11865));
#3109=EDGE_LOOP('',(#11866,#11867,#11868,#11869));
#3110=EDGE_LOOP('',(#11870,#11871,#11872,#11873));
#3111=EDGE_LOOP('',(#11874,#11875,#11876));
#3112=EDGE_LOOP('',(#11877,#11878,#11879,#11880));
#3113=EDGE_LOOP('',(#11881,#11882,#11883,#11884));
#3114=EDGE_LOOP('',(#11885,#11886,#11887,#11888));
#3115=EDGE_LOOP('',(#11889,#11890,#11891,#11892));
#3116=EDGE_LOOP('',(#11893,#11894,#11895,#11896));
#3117=EDGE_LOOP('',(#11897,#11898,#11899));
#3118=EDGE_LOOP('',(#11900,#11901,#11902,#11903,#11904));
#3119=EDGE_LOOP('',(#11905,#11906,#11907,#11908));
#3120=EDGE_LOOP('',(#11909,#11910,#11911,#11912));
#3121=EDGE_LOOP('',(#11913,#11914,#11915,#11916));
#3122=EDGE_LOOP('',(#11917,#11918,#11919,#11920));
#3123=EDGE_LOOP('',(#11921,#11922,#11923,#11924));
#3124=EDGE_LOOP('',(#11925,#11926,#11927,#11928,#11929));
#3125=EDGE_LOOP('',(#11930,#11931,#11932,#11933,#11934,#11935,#11936,#11937,
#11938,#11939,#11940));
#3126=EDGE_LOOP('',(#11941,#11942,#11943,#11944));
#3127=EDGE_LOOP('',(#11945,#11946,#11947));
#3128=EDGE_LOOP('',(#11948,#11949,#11950,#11951,#11952,#11953,#11954,#11955,
#11956,#11957));
#3129=EDGE_LOOP('',(#11958,#11959,#11960,#11961,#11962,#11963,#11964,#11965,
#11966,#11967));
#3130=EDGE_LOOP('',(#11968,#11969,#11970,#11971,#11972,#11973,#11974,#11975,
#11976,#11977,#11978,#11979,#11980,#11981));
#3131=EDGE_LOOP('',(#11982,#11983,#11984,#11985));
#3132=EDGE_LOOP('',(#11986,#11987,#11988,#11989,#11990,#11991,#11992,#11993,
#11994,#11995,#11996,#11997));
#3133=EDGE_LOOP('',(#11998,#11999,#12000,#12001,#12002));
#3134=EDGE_LOOP('',(#12003,#12004,#12005,#12006,#12007,#12008,#12009,#12010));
#3135=EDGE_LOOP('',(#12011,#12012,#12013,#12014,#12015,#12016,#12017,#12018));
#3136=EDGE_LOOP('',(#12019,#12020,#12021,#12022,#12023,#12024,#12025,#12026));
#3137=EDGE_LOOP('',(#12027,#12028,#12029,#12030,#12031,#12032,#12033,#12034));
#3138=EDGE_LOOP('',(#12035,#12036,#12037));
#3139=EDGE_LOOP('',(#12038,#12039,#12040));
#3140=EDGE_LOOP('',(#12041,#12042,#12043));
#3141=EDGE_LOOP('',(#12044,#12045,#12046));
#3142=EDGE_LOOP('',(#12047,#12048,#12049));
#3143=EDGE_LOOP('',(#12050,#12051,#12052));
#3144=EDGE_LOOP('',(#12053,#12054,#12055));
#3145=EDGE_LOOP('',(#12056,#12057,#12058));
#3146=EDGE_LOOP('',(#12059,#12060,#12061));
#3147=EDGE_LOOP('',(#12062,#12063,#12064));
#3148=EDGE_LOOP('',(#12065,#12066,#12067));
#3149=EDGE_LOOP('',(#12068,#12069,#12070));
#3150=EDGE_LOOP('',(#12071,#12072,#12073,#12074,#12075,#12076,#12077,#12078,
#12079,#12080,#12081,#12082,#12083,#12084));
#3151=EDGE_LOOP('',(#12085,#12086,#12087,#12088));
#3152=EDGE_LOOP('',(#12089,#12090,#12091,#12092,#12093,#12094,#12095,#12096,
#12097,#12098,#12099,#12100,#12101,#12102,#12103));
#3153=EDGE_LOOP('',(#12104,#12105,#12106,#12107));
#3154=EDGE_LOOP('',(#12108));
#3155=EDGE_LOOP('',(#12109,#12110,#12111,#12112));
#3156=EDGE_LOOP('',(#12113,#12114,#12115,#12116));
#3157=EDGE_LOOP('',(#12117));
#3158=EDGE_LOOP('',(#12118));
#3159=EDGE_LOOP('',(#12119));
#3160=EDGE_LOOP('',(#12120));
#3161=EDGE_LOOP('',(#12121,#12122,#12123,#12124));
#3162=EDGE_LOOP('',(#12125,#12126,#12127,#12128));
#3163=EDGE_LOOP('',(#12129,#12130,#12131,#12132));
#3164=EDGE_LOOP('',(#12133,#12134,#12135,#12136));
#3165=EDGE_LOOP('',(#12137,#12138,#12139,#12140));
#3166=EDGE_LOOP('',(#12141,#12142,#12143,#12144));
#3167=EDGE_LOOP('',(#12145,#12146,#12147,#12148));
#3168=EDGE_LOOP('',(#12149,#12150,#12151,#12152,#12153,#12154));
#3169=EDGE_LOOP('',(#12155));
#3170=EDGE_LOOP('',(#12156,#12157,#12158,#12159,#12160,#12161));
#3171=EDGE_LOOP('',(#12162));
#3172=EDGE_LOOP('',(#12163,#12164,#12165,#12166));
#3173=EDGE_LOOP('',(#12167,#12168,#12169,#12170));
#3174=EDGE_LOOP('',(#12171,#12172,#12173,#12174));
#3175=EDGE_LOOP('',(#12175,#12176,#12177,#12178));
#3176=EDGE_LOOP('',(#12179,#12180,#12181,#12182));
#3177=EDGE_LOOP('',(#12183,#12184,#12185,#12186));
#3178=EDGE_LOOP('',(#12187,#12188,#12189,#12190));
#3179=EDGE_LOOP('',(#12191,#12192,#12193,#12194,#12195,#12196));
#3180=EDGE_LOOP('',(#12197));
#3181=EDGE_LOOP('',(#12198,#12199,#12200,#12201,#12202,#12203));
#3182=EDGE_LOOP('',(#12204));
#3183=EDGE_LOOP('',(#12205,#12206,#12207,#12208));
#3184=EDGE_LOOP('',(#12209,#12210,#12211,#12212));
#3185=EDGE_LOOP('',(#12213,#12214,#12215,#12216));
#3186=EDGE_LOOP('',(#12217,#12218,#12219,#12220));
#3187=EDGE_LOOP('',(#12221,#12222,#12223,#12224));
#3188=EDGE_LOOP('',(#12225,#12226,#12227,#12228));
#3189=EDGE_LOOP('',(#12229,#12230,#12231,#12232));
#3190=EDGE_LOOP('',(#12233,#12234,#12235,#12236));
#3191=EDGE_LOOP('',(#12237,#12238,#12239,#12240));
#3192=EDGE_LOOP('',(#12241,#12242,#12243,#12244));
#3193=EDGE_LOOP('',(#12245,#12246,#12247,#12248));
#3194=EDGE_LOOP('',(#12249,#12250,#12251,#12252,#12253,#12254,#12255,#12256));
#3195=EDGE_LOOP('',(#12257));
#3196=EDGE_LOOP('',(#12258));
#3197=EDGE_LOOP('',(#12259));
#3198=EDGE_LOOP('',(#12260));
#3199=EDGE_LOOP('',(#12261));
#3200=EDGE_LOOP('',(#12262,#12263,#12264,#12265,#12266,#12267,#12268,#12269));
#3201=EDGE_LOOP('',(#12270));
#3202=EDGE_LOOP('',(#12271));
#3203=EDGE_LOOP('',(#12272));
#3204=EDGE_LOOP('',(#12273));
#3205=EDGE_LOOP('',(#12274));
#3206=EDGE_LOOP('',(#12275,#12276,#12277,#12278));
#3207=EDGE_LOOP('',(#12279,#12280,#12281,#12282));
#3208=EDGE_LOOP('',(#12283,#12284,#12285,#12286));
#3209=EDGE_LOOP('',(#12287,#12288,#12289,#12290));
#3210=EDGE_LOOP('',(#12291,#12292,#12293,#12294));
#3211=EDGE_LOOP('',(#12295,#12296,#12297,#12298));
#3212=EDGE_LOOP('',(#12299,#12300,#12301,#12302));
#3213=EDGE_LOOP('',(#12303,#12304,#12305,#12306));
#3214=EDGE_LOOP('',(#12307,#12308,#12309,#12310));
#3215=EDGE_LOOP('',(#12311,#12312,#12313,#12314));
#3216=EDGE_LOOP('',(#12315,#12316,#12317,#12318));
#3217=EDGE_LOOP('',(#12319,#12320,#12321,#12322));
#3218=EDGE_LOOP('',(#12323,#12324,#12325,#12326));
#3219=EDGE_LOOP('',(#12327,#12328,#12329,#12330));
#3220=EDGE_LOOP('',(#12331,#12332,#12333,#12334));
#3221=EDGE_LOOP('',(#12335,#12336,#12337,#12338));
#3222=EDGE_LOOP('',(#12339,#12340,#12341,#12342));
#3223=EDGE_LOOP('',(#12343,#12344,#12345,#12346));
#3224=EDGE_LOOP('',(#12347,#12348,#12349,#12350));
#3225=EDGE_LOOP('',(#12351,#12352,#12353,#12354));
#3226=EDGE_LOOP('',(#12355,#12356,#12357,#12358));
#3227=EDGE_LOOP('',(#12359,#12360,#12361,#12362));
#3228=EDGE_LOOP('',(#12363,#12364,#12365,#12366));
#3229=EDGE_LOOP('',(#12367,#12368,#12369,#12370));
#3230=EDGE_LOOP('',(#12371,#12372,#12373,#12374));
#3231=EDGE_LOOP('',(#12375,#12376,#12377,#12378));
#3232=EDGE_LOOP('',(#12379,#12380,#12381,#12382,#12383,#12384));
#3233=EDGE_LOOP('',(#12385,#12386,#12387,#12388,#12389,#12390));
#3234=EDGE_LOOP('',(#12391,#12392,#12393,#12394));
#3235=EDGE_LOOP('',(#12395,#12396,#12397,#12398));
#3236=EDGE_LOOP('',(#12399,#12400,#12401,#12402));
#3237=EDGE_LOOP('',(#12403,#12404,#12405,#12406));
#3238=EDGE_LOOP('',(#12407));
#3239=EDGE_LOOP('',(#12408));
#3240=EDGE_LOOP('',(#12409));
#3241=EDGE_LOOP('',(#12410,#12411,#12412,#12413));
#3242=EDGE_LOOP('',(#12414));
#3243=EDGE_LOOP('',(#12415));
#3244=EDGE_LOOP('',(#12416));
#3245=EDGE_LOOP('',(#12417,#12418,#12419,#12420));
#3246=EDGE_LOOP('',(#12421,#12422,#12423,#12424));
#3247=EDGE_LOOP('',(#12425,#12426,#12427,#12428));
#3248=EDGE_LOOP('',(#12429,#12430,#12431,#12432));
#3249=EDGE_LOOP('',(#12433,#12434,#12435,#12436));
#3250=EDGE_LOOP('',(#12437,#12438,#12439,#12440));
#3251=EDGE_LOOP('',(#12441,#12442,#12443,#12444));
#3252=EDGE_LOOP('',(#12445,#12446,#12447,#12448));
#3253=EDGE_LOOP('',(#12449));
#3254=EDGE_LOOP('',(#12450));
#3255=EDGE_LOOP('',(#12451));
#3256=EDGE_LOOP('',(#12452,#12453,#12454,#12455));
#3257=EDGE_LOOP('',(#12456));
#3258=EDGE_LOOP('',(#12457));
#3259=EDGE_LOOP('',(#12458));
#3260=EDGE_LOOP('',(#12459,#12460,#12461,#12462));
#3261=EDGE_LOOP('',(#12463,#12464,#12465,#12466));
#3262=EDGE_LOOP('',(#12467,#12468,#12469,#12470));
#3263=EDGE_LOOP('',(#12471,#12472,#12473,#12474));
#3264=EDGE_LOOP('',(#12475,#12476,#12477,#12478));
#3265=EDGE_LOOP('',(#12479,#12480,#12481,#12482));
#3266=EDGE_LOOP('',(#12483,#12484,#12485,#12486));
#3267=EDGE_LOOP('',(#12487,#12488,#12489,#12490));
#3268=EDGE_LOOP('',(#12491));
#3269=EDGE_LOOP('',(#12492));
#3270=EDGE_LOOP('',(#12493));
#3271=EDGE_LOOP('',(#12494,#12495,#12496,#12497));
#3272=EDGE_LOOP('',(#12498));
#3273=EDGE_LOOP('',(#12499));
#3274=EDGE_LOOP('',(#12500));
#3275=EDGE_LOOP('',(#12501,#12502,#12503,#12504));
#3276=EDGE_LOOP('',(#12505,#12506,#12507,#12508));
#3277=EDGE_LOOP('',(#12509,#12510,#12511,#12512));
#3278=EDGE_LOOP('',(#12513,#12514,#12515,#12516));
#3279=EDGE_LOOP('',(#12517,#12518,#12519,#12520));
#3280=EDGE_LOOP('',(#12521,#12522,#12523,#12524));
#3281=EDGE_LOOP('',(#12525,#12526,#12527,#12528));
#3282=EDGE_LOOP('',(#12529,#12530,#12531,#12532));
#3283=EDGE_LOOP('',(#12533));
#3284=EDGE_LOOP('',(#12534));
#3285=EDGE_LOOP('',(#12535));
#3286=EDGE_LOOP('',(#12536,#12537,#12538,#12539));
#3287=EDGE_LOOP('',(#12540));
#3288=EDGE_LOOP('',(#12541));
#3289=EDGE_LOOP('',(#12542));
#3290=EDGE_LOOP('',(#12543,#12544,#12545,#12546));
#3291=EDGE_LOOP('',(#12547,#12548,#12549,#12550));
#3292=EDGE_LOOP('',(#12551,#12552,#12553,#12554));
#3293=EDGE_LOOP('',(#12555,#12556,#12557,#12558));
#3294=EDGE_LOOP('',(#12559,#12560,#12561,#12562));
#3295=EDGE_LOOP('',(#12563,#12564,#12565,#12566));
#3296=EDGE_LOOP('',(#12567,#12568,#12569,#12570));
#3297=EDGE_LOOP('',(#12571,#12572,#12573,#12574));
#3298=EDGE_LOOP('',(#12575,#12576,#12577,#12578));
#3299=EDGE_LOOP('',(#12579,#12580,#12581,#12582));
#3300=EDGE_LOOP('',(#12583,#12584,#12585,#12586));
#3301=EDGE_LOOP('',(#12587,#12588,#12589,#12590));
#3302=EDGE_LOOP('',(#12591,#12592,#12593,#12594));
#3303=EDGE_LOOP('',(#12595,#12596,#12597,#12598));
#3304=EDGE_LOOP('',(#12599,#12600,#12601,#12602));
#3305=EDGE_LOOP('',(#12603,#12604,#12605,#12606));
#3306=EDGE_LOOP('',(#12607,#12608,#12609,#12610));
#3307=EDGE_LOOP('',(#12611,#12612,#12613,#12614));
#3308=EDGE_LOOP('',(#12615,#12616,#12617,#12618));
#3309=EDGE_LOOP('',(#12619,#12620,#12621,#12622));
#3310=EDGE_LOOP('',(#12623,#12624,#12625,#12626));
#3311=EDGE_LOOP('',(#12627,#12628,#12629,#12630));
#3312=EDGE_LOOP('',(#12631,#12632,#12633,#12634));
#3313=EDGE_LOOP('',(#12635,#12636,#12637,#12638));
#3314=EDGE_LOOP('',(#12639,#12640,#12641,#12642));
#3315=EDGE_LOOP('',(#12643,#12644,#12645,#12646));
#3316=EDGE_LOOP('',(#12647,#12648,#12649,#12650));
#3317=EDGE_LOOP('',(#12651,#12652,#12653,#12654));
#3318=EDGE_LOOP('',(#12655,#12656,#12657,#12658));
#3319=EDGE_LOOP('',(#12659,#12660,#12661,#12662));
#3320=EDGE_LOOP('',(#12663,#12664,#12665,#12666));
#3321=EDGE_LOOP('',(#12667,#12668,#12669,#12670));
#3322=EDGE_LOOP('',(#12671,#12672,#12673,#12674));
#3323=EDGE_LOOP('',(#12675,#12676,#12677,#12678));
#3324=EDGE_LOOP('',(#12679,#12680,#12681,#12682));
#3325=EDGE_LOOP('',(#12683,#12684,#12685,#12686));
#3326=EDGE_LOOP('',(#12687,#12688,#12689,#12690));
#3327=EDGE_LOOP('',(#12691,#12692,#12693,#12694));
#3328=EDGE_LOOP('',(#12695,#12696,#12697,#12698));
#3329=EDGE_LOOP('',(#12699));
#3330=EDGE_LOOP('',(#12700));
#3331=EDGE_LOOP('',(#12701));
#3332=EDGE_LOOP('',(#12702));
#3333=EDGE_LOOP('',(#12703,#12704,#12705,#12706));
#3334=EDGE_LOOP('',(#12707));
#3335=EDGE_LOOP('',(#12708));
#3336=EDGE_LOOP('',(#12709));
#3337=EDGE_LOOP('',(#12710));
#3338=EDGE_LOOP('',(#12711,#12712,#12713,#12714));
#3339=EDGE_LOOP('',(#12715,#12716,#12717,#12718));
#3340=EDGE_LOOP('',(#12719,#12720,#12721,#12722));
#3341=EDGE_LOOP('',(#12723,#12724,#12725,#12726));
#3342=EDGE_LOOP('',(#12727,#12728,#12729,#12730));
#3343=EDGE_LOOP('',(#12731,#12732,#12733,#12734));
#3344=EDGE_LOOP('',(#12735,#12736,#12737,#12738));
#3345=EDGE_LOOP('',(#12739,#12740,#12741,#12742));
#3346=EDGE_LOOP('',(#12743,#12744,#12745,#12746));
#3347=EDGE_LOOP('',(#12747,#12748,#12749,#12750));
#3348=EDGE_LOOP('',(#12751,#12752,#12753,#12754));
#3349=EDGE_LOOP('',(#12755,#12756,#12757,#12758));
#3350=EDGE_LOOP('',(#12759,#12760,#12761,#12762));
#3351=EDGE_LOOP('',(#12763,#12764,#12765,#12766));
#3352=EDGE_LOOP('',(#12767,#12768,#12769,#12770));
#3353=EDGE_LOOP('',(#12771));
#3354=EDGE_LOOP('',(#12772));
#3355=EDGE_LOOP('',(#12773));
#3356=EDGE_LOOP('',(#12774));
#3357=EDGE_LOOP('',(#12775));
#3358=EDGE_LOOP('',(#12776));
#3359=EDGE_LOOP('',(#12777,#12778,#12779,#12780));
#3360=EDGE_LOOP('',(#12781));
#3361=EDGE_LOOP('',(#12782));
#3362=EDGE_LOOP('',(#12783));
#3363=EDGE_LOOP('',(#12784));
#3364=EDGE_LOOP('',(#12785));
#3365=EDGE_LOOP('',(#12786));
#3366=EDGE_LOOP('',(#12787,#12788,#12789,#12790));
#3367=EDGE_LOOP('',(#12791,#12792,#12793,#12794));
#3368=EDGE_LOOP('',(#12795,#12796,#12797,#12798));
#3369=EDGE_LOOP('',(#12799,#12800,#12801,#12802));
#3370=EDGE_LOOP('',(#12803,#12804,#12805,#12806));
#3371=EDGE_LOOP('',(#12807,#12808,#12809,#12810));
#3372=EDGE_LOOP('',(#12811,#12812,#12813,#12814));
#3373=EDGE_LOOP('',(#12815,#12816,#12817,#12818,#12819,#12820,#12821));
#3374=EDGE_LOOP('',(#12822,#12823,#12824,#12825,#12826,#12827,#12828));
#3375=EDGE_LOOP('',(#12829,#12830,#12831,#12832));
#3376=EDGE_LOOP('',(#12833,#12834,#12835,#12836));
#3377=EDGE_LOOP('',(#12837,#12838,#12839,#12840));
#3378=EDGE_LOOP('',(#12841,#12842,#12843,#12844));
#3379=EDGE_LOOP('',(#12845,#12846,#12847,#12848));
#3380=EDGE_LOOP('',(#12849,#12850,#12851,#12852));
#3381=EDGE_LOOP('',(#12853,#12854,#12855,#12856));
#3382=EDGE_LOOP('',(#12857,#12858,#12859,#12860,#12861,#12862,#12863));
#3383=EDGE_LOOP('',(#12864,#12865,#12866,#12867,#12868,#12869,#12870));
#3384=EDGE_LOOP('',(#12871,#12872,#12873,#12874));
#3385=EDGE_LOOP('',(#12875,#12876,#12877,#12878));
#3386=EDGE_LOOP('',(#12879,#12880,#12881,#12882));
#3387=EDGE_LOOP('',(#12883,#12884,#12885,#12886));
#3388=EDGE_LOOP('',(#12887,#12888,#12889,#12890));
#3389=EDGE_LOOP('',(#12891,#12892,#12893,#12894));
#3390=EDGE_LOOP('',(#12895,#12896,#12897,#12898));
#3391=EDGE_LOOP('',(#12899,#12900,#12901,#12902,#12903,#12904,#12905));
#3392=EDGE_LOOP('',(#12906,#12907,#12908,#12909,#12910,#12911,#12912));
#3393=EDGE_LOOP('',(#12913,#12914,#12915,#12916));
#3394=EDGE_LOOP('',(#12917,#12918,#12919,#12920));
#3395=EDGE_LOOP('',(#12921,#12922,#12923,#12924));
#3396=EDGE_LOOP('',(#12925,#12926,#12927,#12928));
#3397=EDGE_LOOP('',(#12929,#12930,#12931,#12932));
#3398=EDGE_LOOP('',(#12933,#12934,#12935,#12936));
#3399=EDGE_LOOP('',(#12937,#12938,#12939,#12940));
#3400=EDGE_LOOP('',(#12941,#12942,#12943,#12944,#12945,#12946,#12947));
#3401=EDGE_LOOP('',(#12948,#12949,#12950,#12951,#12952,#12953,#12954));
#3402=EDGE_LOOP('',(#12955,#12956,#12957,#12958));
#3403=EDGE_LOOP('',(#12959,#12960,#12961,#12962));
#3404=EDGE_LOOP('',(#12963,#12964,#12965,#12966));
#3405=EDGE_LOOP('',(#12967,#12968,#12969,#12970));
#3406=EDGE_LOOP('',(#12971,#12972,#12973,#12974));
#3407=EDGE_LOOP('',(#12975,#12976,#12977,#12978));
#3408=EDGE_LOOP('',(#12979,#12980,#12981,#12982));
#3409=EDGE_LOOP('',(#12983,#12984,#12985,#12986,#12987,#12988,#12989));
#3410=EDGE_LOOP('',(#12990,#12991,#12992,#12993,#12994,#12995,#12996));
#3411=EDGE_LOOP('',(#12997,#12998,#12999,#13000));
#3412=EDGE_LOOP('',(#13001,#13002,#13003,#13004));
#3413=EDGE_LOOP('',(#13005,#13006,#13007,#13008));
#3414=EDGE_LOOP('',(#13009,#13010,#13011,#13012));
#3415=EDGE_LOOP('',(#13013,#13014,#13015,#13016));
#3416=EDGE_LOOP('',(#13017,#13018,#13019,#13020));
#3417=EDGE_LOOP('',(#13021,#13022,#13023,#13024));
#3418=EDGE_LOOP('',(#13025,#13026,#13027,#13028,#13029,#13030,#13031));
#3419=EDGE_LOOP('',(#13032,#13033,#13034,#13035,#13036,#13037,#13038));
#3420=EDGE_LOOP('',(#13039,#13040,#13041,#13042));
#3421=EDGE_LOOP('',(#13043,#13044,#13045,#13046));
#3422=EDGE_LOOP('',(#13047,#13048,#13049,#13050));
#3423=EDGE_LOOP('',(#13051,#13052,#13053,#13054));
#3424=EDGE_LOOP('',(#13055,#13056,#13057,#13058));
#3425=EDGE_LOOP('',(#13059,#13060,#13061,#13062));
#3426=EDGE_LOOP('',(#13063,#13064,#13065,#13066));
#3427=EDGE_LOOP('',(#13067,#13068,#13069,#13070,#13071,#13072,#13073));
#3428=EDGE_LOOP('',(#13074,#13075,#13076,#13077,#13078,#13079,#13080));
#3429=EDGE_LOOP('',(#13081,#13082,#13083,#13084));
#3430=EDGE_LOOP('',(#13085,#13086,#13087,#13088));
#3431=EDGE_LOOP('',(#13089,#13090,#13091,#13092));
#3432=EDGE_LOOP('',(#13093,#13094,#13095,#13096));
#3433=EDGE_LOOP('',(#13097,#13098,#13099,#13100));
#3434=EDGE_LOOP('',(#13101,#13102,#13103,#13104));
#3435=EDGE_LOOP('',(#13105,#13106,#13107,#13108));
#3436=EDGE_LOOP('',(#13109,#13110,#13111,#13112,#13113,#13114,#13115));
#3437=EDGE_LOOP('',(#13116,#13117,#13118,#13119,#13120,#13121,#13122));
#3438=EDGE_LOOP('',(#13123,#13124,#13125,#13126));
#3439=EDGE_LOOP('',(#13127,#13128,#13129,#13130));
#3440=EDGE_LOOP('',(#13131,#13132,#13133,#13134));
#3441=EDGE_LOOP('',(#13135,#13136,#13137,#13138));
#3442=EDGE_LOOP('',(#13139,#13140,#13141,#13142));
#3443=EDGE_LOOP('',(#13143,#13144,#13145,#13146));
#3444=EDGE_LOOP('',(#13147,#13148,#13149,#13150));
#3445=EDGE_LOOP('',(#13151,#13152,#13153,#13154,#13155,#13156,#13157));
#3446=EDGE_LOOP('',(#13158,#13159,#13160,#13161,#13162,#13163,#13164));
#3447=EDGE_LOOP('',(#13165,#13166,#13167,#13168));
#3448=EDGE_LOOP('',(#13169,#13170,#13171,#13172));
#3449=EDGE_LOOP('',(#13173,#13174,#13175,#13176));
#3450=EDGE_LOOP('',(#13177,#13178,#13179,#13180));
#3451=EDGE_LOOP('',(#13181,#13182,#13183,#13184));
#3452=EDGE_LOOP('',(#13185,#13186,#13187,#13188));
#3453=EDGE_LOOP('',(#13189,#13190,#13191,#13192));
#3454=EDGE_LOOP('',(#13193,#13194,#13195,#13196,#13197,#13198,#13199));
#3455=EDGE_LOOP('',(#13200,#13201,#13202,#13203,#13204,#13205,#13206));
#3456=EDGE_LOOP('',(#13207,#13208,#13209,#13210));
#3457=EDGE_LOOP('',(#13211,#13212,#13213,#13214));
#3458=EDGE_LOOP('',(#13215,#13216,#13217,#13218));
#3459=EDGE_LOOP('',(#13219,#13220,#13221,#13222));
#3460=EDGE_LOOP('',(#13223,#13224,#13225,#13226));
#3461=EDGE_LOOP('',(#13227,#13228,#13229,#13230));
#3462=EDGE_LOOP('',(#13231,#13232,#13233,#13234));
#3463=EDGE_LOOP('',(#13235,#13236,#13237,#13238,#13239,#13240,#13241));
#3464=EDGE_LOOP('',(#13242,#13243,#13244,#13245,#13246,#13247,#13248));
#3465=EDGE_LOOP('',(#13249,#13250,#13251,#13252));
#3466=EDGE_LOOP('',(#13253,#13254,#13255,#13256));
#3467=EDGE_LOOP('',(#13257,#13258,#13259,#13260));
#3468=EDGE_LOOP('',(#13261,#13262,#13263,#13264));
#3469=EDGE_LOOP('',(#13265,#13266,#13267,#13268));
#3470=EDGE_LOOP('',(#13269));
#3471=EDGE_LOOP('',(#13270));
#3472=EDGE_LOOP('',(#13271));
#3473=EDGE_LOOP('',(#13272));
#3474=EDGE_LOOP('',(#13273,#13274,#13275,#13276));
#3475=EDGE_LOOP('',(#13277));
#3476=EDGE_LOOP('',(#13278));
#3477=EDGE_LOOP('',(#13279));
#3478=EDGE_LOOP('',(#13280));
#3479=EDGE_LOOP('',(#13281,#13282,#13283,#13284));
#3480=EDGE_LOOP('',(#13285,#13286,#13287,#13288));
#3481=EDGE_LOOP('',(#13289,#13290,#13291,#13292));
#3482=EDGE_LOOP('',(#13293,#13294,#13295,#13296));
#3483=EDGE_LOOP('',(#13297,#13298,#13299,#13300));
#3484=EDGE_LOOP('',(#13301,#13302,#13303,#13304));
#3485=EDGE_LOOP('',(#13305,#13306,#13307,#13308));
#3486=EDGE_LOOP('',(#13309,#13310,#13311,#13312));
#3487=EDGE_LOOP('',(#13313,#13314,#13315,#13316));
#3488=EDGE_LOOP('',(#13317,#13318,#13319,#13320));
#3489=EDGE_LOOP('',(#13321,#13322,#13323,#13324));
#3490=EDGE_LOOP('',(#13325,#13326,#13327,#13328));
#3491=EDGE_LOOP('',(#13329,#13330,#13331,#13332));
#3492=EDGE_LOOP('',(#13333,#13334,#13335,#13336));
#3493=EDGE_LOOP('',(#13337,#13338,#13339,#13340));
#3494=EDGE_LOOP('',(#13341,#13342,#13343,#13344));
#3495=EDGE_LOOP('',(#13345,#13346,#13347,#13348));
#3496=EDGE_LOOP('',(#13349,#13350,#13351,#13352));
#3497=EDGE_LOOP('',(#13353,#13354,#13355,#13356));
#3498=EDGE_LOOP('',(#13357,#13358,#13359,#13360));
#3499=EDGE_LOOP('',(#13361,#13362,#13363,#13364));
#3500=EDGE_LOOP('',(#13365,#13366,#13367,#13368));
#3501=EDGE_LOOP('',(#13369,#13370,#13371,#13372));
#3502=EDGE_LOOP('',(#13373,#13374,#13375,#13376));
#3503=EDGE_LOOP('',(#13377,#13378,#13379,#13380));
#3504=EDGE_LOOP('',(#13381,#13382,#13383,#13384));
#3505=EDGE_LOOP('',(#13385,#13386,#13387,#13388));
#3506=EDGE_LOOP('',(#13389,#13390,#13391,#13392));
#3507=EDGE_LOOP('',(#13393,#13394,#13395,#13396));
#3508=EDGE_LOOP('',(#13397,#13398,#13399,#13400));
#3509=EDGE_LOOP('',(#13401,#13402,#13403,#13404));
#3510=EDGE_LOOP('',(#13405,#13406,#13407,#13408));
#3511=EDGE_LOOP('',(#13409,#13410,#13411,#13412));
#3512=EDGE_LOOP('',(#13413,#13414,#13415,#13416));
#3513=EDGE_LOOP('',(#13417,#13418,#13419,#13420));
#3514=EDGE_LOOP('',(#13421,#13422,#13423,#13424));
#3515=EDGE_LOOP('',(#13425,#13426,#13427,#13428));
#3516=EDGE_LOOP('',(#13429,#13430,#13431,#13432));
#3517=EDGE_LOOP('',(#13433,#13434,#13435,#13436));
#3518=EDGE_LOOP('',(#13437,#13438,#13439,#13440));
#3519=EDGE_LOOP('',(#13441,#13442,#13443,#13444));
#3520=EDGE_LOOP('',(#13445,#13446,#13447,#13448));
#3521=EDGE_LOOP('',(#13449,#13450,#13451,#13452));
#3522=EDGE_LOOP('',(#13453,#13454,#13455,#13456));
#3523=EDGE_LOOP('',(#13457,#13458,#13459,#13460));
#3524=EDGE_LOOP('',(#13461,#13462,#13463,#13464));
#3525=EDGE_LOOP('',(#13465,#13466,#13467,#13468));
#3526=EDGE_LOOP('',(#13469,#13470,#13471,#13472));
#3527=EDGE_LOOP('',(#13473,#13474,#13475,#13476));
#3528=EDGE_LOOP('',(#13477,#13478,#13479,#13480));
#3529=EDGE_LOOP('',(#13481,#13482,#13483,#13484));
#3530=EDGE_LOOP('',(#13485,#13486,#13487,#13488));
#3531=EDGE_LOOP('',(#13489,#13490,#13491,#13492));
#3532=EDGE_LOOP('',(#13493,#13494,#13495,#13496));
#3533=EDGE_LOOP('',(#13497,#13498,#13499,#13500));
#3534=EDGE_LOOP('',(#13501,#13502,#13503,#13504));
#3535=EDGE_LOOP('',(#13505,#13506,#13507,#13508));
#3536=EDGE_LOOP('',(#13509,#13510,#13511,#13512));
#3537=EDGE_LOOP('',(#13513,#13514,#13515,#13516));
#3538=EDGE_LOOP('',(#13517,#13518,#13519,#13520));
#3539=EDGE_LOOP('',(#13521,#13522,#13523,#13524));
#3540=EDGE_LOOP('',(#13525,#13526,#13527,#13528));
#3541=EDGE_LOOP('',(#13529,#13530,#13531,#13532));
#3542=EDGE_LOOP('',(#13533,#13534,#13535,#13536));
#3543=EDGE_LOOP('',(#13537,#13538,#13539,#13540));
#3544=EDGE_LOOP('',(#13541,#13542,#13543,#13544));
#3545=EDGE_LOOP('',(#13545,#13546,#13547,#13548));
#3546=EDGE_LOOP('',(#13549,#13550,#13551,#13552));
#3547=EDGE_LOOP('',(#13553,#13554,#13555,#13556));
#3548=EDGE_LOOP('',(#13557,#13558,#13559,#13560));
#3549=EDGE_LOOP('',(#13561,#13562,#13563,#13564));
#3550=EDGE_LOOP('',(#13565,#13566,#13567,#13568));
#3551=EDGE_LOOP('',(#13569,#13570,#13571,#13572));
#3552=EDGE_LOOP('',(#13573,#13574,#13575,#13576));
#3553=EDGE_LOOP('',(#13577,#13578,#13579,#13580));
#3554=EDGE_LOOP('',(#13581,#13582,#13583,#13584));
#3555=EDGE_LOOP('',(#13585,#13586,#13587,#13588));
#3556=EDGE_LOOP('',(#13589,#13590,#13591,#13592));
#3557=EDGE_LOOP('',(#13593,#13594,#13595,#13596));
#3558=EDGE_LOOP('',(#13597,#13598,#13599,#13600));
#3559=EDGE_LOOP('',(#13601,#13602,#13603,#13604));
#3560=EDGE_LOOP('',(#13605,#13606,#13607,#13608));
#3561=EDGE_LOOP('',(#13609,#13610,#13611,#13612));
#3562=EDGE_LOOP('',(#13613,#13614,#13615,#13616));
#3563=EDGE_LOOP('',(#13617,#13618,#13619,#13620));
#3564=EDGE_LOOP('',(#13621,#13622,#13623,#13624));
#3565=EDGE_LOOP('',(#13625,#13626,#13627,#13628));
#3566=EDGE_LOOP('',(#13629,#13630,#13631,#13632));
#3567=EDGE_LOOP('',(#13633,#13634,#13635,#13636));
#3568=EDGE_LOOP('',(#13637,#13638,#13639,#13640));
#3569=EDGE_LOOP('',(#13641,#13642,#13643,#13644));
#3570=EDGE_LOOP('',(#13645,#13646,#13647,#13648));
#3571=EDGE_LOOP('',(#13649,#13650,#13651,#13652));
#3572=EDGE_LOOP('',(#13653,#13654,#13655,#13656));
#3573=EDGE_LOOP('',(#13657,#13658,#13659,#13660));
#3574=EDGE_LOOP('',(#13661,#13662,#13663,#13664));
#3575=EDGE_LOOP('',(#13665,#13666,#13667,#13668));
#3576=EDGE_LOOP('',(#13669,#13670,#13671,#13672));
#3577=EDGE_LOOP('',(#13673,#13674,#13675,#13676));
#3578=EDGE_LOOP('',(#13677,#13678,#13679,#13680));
#3579=EDGE_LOOP('',(#13681,#13682,#13683,#13684));
#3580=EDGE_LOOP('',(#13685,#13686,#13687,#13688));
#3581=EDGE_LOOP('',(#13689,#13690,#13691,#13692));
#3582=EDGE_LOOP('',(#13693,#13694,#13695,#13696));
#3583=EDGE_LOOP('',(#13697,#13698,#13699,#13700));
#3584=EDGE_LOOP('',(#13701,#13702,#13703,#13704));
#3585=EDGE_LOOP('',(#13705,#13706,#13707,#13708));
#3586=EDGE_LOOP('',(#13709,#13710,#13711,#13712));
#3587=EDGE_LOOP('',(#13713,#13714,#13715,#13716));
#3588=EDGE_LOOP('',(#13717,#13718,#13719,#13720));
#3589=EDGE_LOOP('',(#13721,#13722,#13723,#13724));
#3590=EDGE_LOOP('',(#13725,#13726,#13727,#13728));
#3591=EDGE_LOOP('',(#13729,#13730,#13731,#13732));
#3592=EDGE_LOOP('',(#13733,#13734,#13735,#13736));
#3593=EDGE_LOOP('',(#13737,#13738,#13739,#13740));
#3594=EDGE_LOOP('',(#13741,#13742,#13743,#13744));
#3595=EDGE_LOOP('',(#13745,#13746,#13747,#13748));
#3596=EDGE_LOOP('',(#13749,#13750,#13751,#13752));
#3597=EDGE_LOOP('',(#13753,#13754,#13755,#13756));
#3598=EDGE_LOOP('',(#13757,#13758,#13759,#13760));
#3599=EDGE_LOOP('',(#13761,#13762,#13763,#13764));
#3600=EDGE_LOOP('',(#13765,#13766,#13767,#13768));
#3601=EDGE_LOOP('',(#13769,#13770,#13771,#13772));
#3602=EDGE_LOOP('',(#13773,#13774,#13775,#13776));
#3603=EDGE_LOOP('',(#13777,#13778,#13779,#13780));
#3604=EDGE_LOOP('',(#13781,#13782,#13783,#13784));
#3605=EDGE_LOOP('',(#13785,#13786,#13787,#13788));
#3606=EDGE_LOOP('',(#13789,#13790,#13791,#13792));
#3607=EDGE_LOOP('',(#13793,#13794,#13795,#13796));
#3608=EDGE_LOOP('',(#13797,#13798,#13799,#13800));
#3609=EDGE_LOOP('',(#13801,#13802,#13803,#13804));
#3610=EDGE_LOOP('',(#13805,#13806,#13807,#13808));
#3611=EDGE_LOOP('',(#13809,#13810,#13811,#13812));
#3612=EDGE_LOOP('',(#13813,#13814,#13815,#13816));
#3613=EDGE_LOOP('',(#13817,#13818,#13819,#13820));
#3614=EDGE_LOOP('',(#13821,#13822,#13823,#13824));
#3615=EDGE_LOOP('',(#13825,#13826,#13827,#13828,#13829));
#3616=EDGE_LOOP('',(#13830,#13831,#13832,#13833,#13834,#13835,#13836,#13837,
#13838));
#3617=EDGE_LOOP('',(#13839,#13840,#13841,#13842));
#3618=EDGE_LOOP('',(#13843,#13844,#13845,#13846,#13847));
#3619=EDGE_LOOP('',(#13848));
#3620=EDGE_LOOP('',(#13849));
#3621=EDGE_LOOP('',(#13850));
#3622=EDGE_LOOP('',(#13851,#13852,#13853));
#3623=EDGE_LOOP('',(#13854,#13855,#13856));
#3624=EDGE_LOOP('',(#13857,#13858,#13859));
#3625=EDGE_LOOP('',(#13860,#13861,#13862));
#3626=EDGE_LOOP('',(#13863,#13864,#13865));
#3627=EDGE_LOOP('',(#13866,#13867,#13868));
#3628=EDGE_LOOP('',(#13869,#13870,#13871,#13872,#13873,#13874));
#3629=EDGE_LOOP('',(#13875,#13876,#13877));
#3630=EDGE_LOOP('',(#13878,#13879,#13880));
#3631=EDGE_LOOP('',(#13881,#13882,#13883));
#3632=EDGE_LOOP('',(#13884,#13885,#13886));
#3633=EDGE_LOOP('',(#13887,#13888,#13889));
#3634=EDGE_LOOP('',(#13890,#13891,#13892));
#3635=EDGE_LOOP('',(#13893,#13894,#13895,#13896,#13897,#13898));
#3636=EDGE_LOOP('',(#13899,#13900,#13901,#13902,#13903,#13904));
#3637=EDGE_LOOP('',(#13905,#13906,#13907,#13908,#13909,#13910));
#3638=EDGE_LOOP('',(#13911,#13912,#13913,#13914,#13915,#13916));
#3639=EDGE_LOOP('',(#13917,#13918,#13919,#13920,#13921,#13922));
#3640=EDGE_LOOP('',(#13923,#13924,#13925,#13926,#13927,#13928));
#3641=EDGE_LOOP('',(#13929,#13930,#13931,#13932));
#3642=EDGE_LOOP('',(#13933,#13934,#13935,#13936));
#3643=EDGE_LOOP('',(#13937));
#3644=EDGE_LOOP('',(#13938));
#3645=EDGE_LOOP('',(#13939));
#3646=EDGE_LOOP('',(#13940));
#3647=EDGE_LOOP('',(#13941,#13942,#13943,#13944,#13945));
#3648=EDGE_LOOP('',(#13946,#13947,#13948,#13949,#13950,#13951));
#3649=EDGE_LOOP('',(#13952,#13953,#13954,#13955));
#3650=EDGE_LOOP('',(#13956,#13957,#13958,#13959,#13960));
#3651=EDGE_LOOP('',(#13961,#13962,#13963,#13964,#13965,#13966));
#3652=EDGE_LOOP('',(#13967,#13968,#13969,#13970,#13971,#13972));
#3653=EDGE_LOOP('',(#13973,#13974,#13975,#13976,#13977,#13978));
#3654=EDGE_LOOP('',(#13979,#13980,#13981,#13982,#13983,#13984));
#3655=EDGE_LOOP('',(#13985,#13986,#13987,#13988,#13989,#13990));
#3656=EDGE_LOOP('',(#13991,#13992,#13993,#13994,#13995,#13996));
#3657=EDGE_LOOP('',(#13997,#13998,#13999,#14000,#14001,#14002));
#3658=EDGE_LOOP('',(#14003));
#3659=EDGE_LOOP('',(#14004,#14005,#14006,#14007,#14008,#14009));
#3660=EDGE_LOOP('',(#14010));
#3661=EDGE_LOOP('',(#14011,#14012,#14013));
#3662=EDGE_LOOP('',(#14014,#14015,#14016));
#3663=EDGE_LOOP('',(#14017,#14018,#14019));
#3664=EDGE_LOOP('',(#14020,#14021,#14022));
#3665=EDGE_LOOP('',(#14023,#14024,#14025));
#3666=EDGE_LOOP('',(#14026,#14027,#14028));
#3667=EDGE_LOOP('',(#14029,#14030,#14031));
#3668=EDGE_LOOP('',(#14032,#14033,#14034));
#3669=EDGE_LOOP('',(#14035,#14036,#14037));
#3670=EDGE_LOOP('',(#14038,#14039,#14040));
#3671=EDGE_LOOP('',(#14041,#14042,#14043));
#3672=EDGE_LOOP('',(#14044,#14045,#14046));
#3673=LINE('',#21314,#5077);
#3674=LINE('',#21316,#5078);
#3675=LINE('',#21318,#5079);
#3676=LINE('',#21319,#5080);
#3677=LINE('',#21322,#5081);
#3678=LINE('',#21324,#5082);
#3679=LINE('',#21325,#5083);
#3680=LINE('',#21328,#5084);
#3681=LINE('',#21330,#5085);
#3682=LINE('',#21331,#5086);
#3683=LINE('',#21333,#5087);
#3684=LINE('',#21334,#5088);
#3685=LINE('',#21338,#5089);
#3686=LINE('',#21340,#5090);
#3687=LINE('',#21342,#5091);
#3688=LINE('',#21343,#5092);
#3689=LINE('',#21347,#5093);
#3690=LINE('',#21349,#5094);
#3691=LINE('',#21351,#5095);
#3692=LINE('',#21352,#5096);
#3693=LINE('',#21354,#5097);
#3694=LINE('',#21355,#5098);
#3695=LINE('',#21357,#5099);
#3696=LINE('',#21359,#5100);
#3697=LINE('',#21364,#5101);
#3698=LINE('',#21366,#5102);
#3699=LINE('',#21368,#5103);
#3700=LINE('',#21369,#5104);
#3701=LINE('',#21372,#5105);
#3702=LINE('',#21374,#5106);
#3703=LINE('',#21375,#5107);
#3704=LINE('',#21380,#5108);
#3705=LINE('',#21384,#5109);
#3706=LINE('',#21386,#5110);
#3707=LINE('',#21387,#5111);
#3708=LINE('',#21390,#5112);
#3709=LINE('',#21392,#5113);
#3710=LINE('',#21393,#5114);
#3711=LINE('',#21395,#5115);
#3712=LINE('',#21396,#5116);
#3713=LINE('',#21402,#5117);
#3714=LINE('',#21404,#5118);
#3715=LINE('',#21406,#5119);
#3716=LINE('',#21407,#5120);
#3717=LINE('',#21410,#5121);
#3718=LINE('',#21412,#5122);
#3719=LINE('',#21413,#5123);
#3720=LINE('',#21419,#5124);
#3721=LINE('',#21422,#5125);
#3722=LINE('',#21424,#5126);
#3723=LINE('',#21425,#5127);
#3724=LINE('',#21428,#5128);
#3725=LINE('',#21430,#5129);
#3726=LINE('',#21431,#5130);
#3727=LINE('',#21433,#5131);
#3728=LINE('',#21434,#5132);
#3729=LINE('',#21441,#5133);
#3730=LINE('',#21447,#5134);
#3731=LINE('',#21453,#5135);
#3732=LINE('',#21459,#5136);
#3733=LINE('',#21465,#5137);
#3734=LINE('',#21471,#5138);
#3735=LINE('',#21476,#5139);
#3736=LINE('',#21478,#5140);
#3737=LINE('',#21480,#5141);
#3738=LINE('',#21481,#5142);
#3739=LINE('',#21485,#5143);
#3740=LINE('',#21487,#5144);
#3741=LINE('',#21489,#5145);
#3742=LINE('',#21490,#5146);
#3743=LINE('',#21492,#5147);
#3744=LINE('',#21493,#5148);
#3745=LINE('',#21495,#5149);
#3746=LINE('',#21497,#5150);
#3747=LINE('',#21503,#5151);
#3748=LINE('',#21509,#5152);
#3749=LINE('',#21515,#5153);
#3750=LINE('',#21521,#5154);
#3751=LINE('',#21527,#5155);
#3752=LINE('',#21532,#5156);
#3753=LINE('',#21534,#5157);
#3754=LINE('',#21536,#5158);
#3755=LINE('',#21537,#5159);
#3756=LINE('',#21540,#5160);
#3757=LINE('',#21542,#5161);
#3758=LINE('',#21543,#5162);
#3759=LINE('',#21546,#5163);
#3760=LINE('',#21548,#5164);
#3761=LINE('',#21549,#5165);
#3762=LINE('',#21551,#5166);
#3763=LINE('',#21552,#5167);
#3764=LINE('',#21559,#5168);
#3765=LINE('',#21565,#5169);
#3766=LINE('',#21571,#5170);
#3767=LINE('',#21577,#5171);
#3768=LINE('',#21583,#5172);
#3769=LINE('',#21588,#5173);
#3770=LINE('',#21590,#5174);
#3771=LINE('',#21592,#5175);
#3772=LINE('',#21593,#5176);
#3773=LINE('',#21596,#5177);
#3774=LINE('',#21598,#5178);
#3775=LINE('',#21599,#5179);
#3776=LINE('',#21602,#5180);
#3777=LINE('',#21604,#5181);
#3778=LINE('',#21605,#5182);
#3779=LINE('',#21607,#5183);
#3780=LINE('',#21608,#5184);
#3781=LINE('',#21614,#5185);
#3782=LINE('',#21616,#5186);
#3783=LINE('',#21618,#5187);
#3784=LINE('',#21619,#5188);
#3785=LINE('',#21622,#5189);
#3786=LINE('',#21624,#5190);
#3787=LINE('',#21625,#5191);
#3788=LINE('',#21628,#5192);
#3789=LINE('',#21630,#5193);
#3790=LINE('',#21631,#5194);
#3791=LINE('',#21633,#5195);
#3792=LINE('',#21634,#5196);
#3793=LINE('',#21640,#5197);
#3794=LINE('',#21642,#5198);
#3795=LINE('',#21644,#5199);
#3796=LINE('',#21645,#5200);
#3797=LINE('',#21648,#5201);
#3798=LINE('',#21650,#5202);
#3799=LINE('',#21651,#5203);
#3800=LINE('',#21654,#5204);
#3801=LINE('',#21656,#5205);
#3802=LINE('',#21657,#5206);
#3803=LINE('',#21659,#5207);
#3804=LINE('',#21660,#5208);
#3805=LINE('',#21666,#5209);
#3806=LINE('',#21668,#5210);
#3807=LINE('',#21670,#5211);
#3808=LINE('',#21671,#5212);
#3809=LINE('',#21674,#5213);
#3810=LINE('',#21676,#5214);
#3811=LINE('',#21677,#5215);
#3812=LINE('',#21680,#5216);
#3813=LINE('',#21682,#5217);
#3814=LINE('',#21683,#5218);
#3815=LINE('',#21685,#5219);
#3816=LINE('',#21686,#5220);
#3817=LINE('',#21694,#5221);
#3818=LINE('',#21700,#5222);
#3819=LINE('',#21706,#5223);
#3820=LINE('',#21712,#5224);
#3821=LINE('',#21718,#5225);
#3822=LINE('',#21724,#5226);
#3823=LINE('',#21730,#5227);
#3824=LINE('',#21736,#5228);
#3825=LINE('',#21742,#5229);
#3826=LINE('',#21748,#5230);
#3827=LINE('',#21754,#5231);
#3828=LINE('',#21760,#5232);
#3829=LINE('',#21766,#5233);
#3830=LINE('',#21772,#5234);
#3831=LINE('',#21778,#5235);
#3832=LINE('',#21784,#5236);
#3833=LINE('',#21790,#5237);
#3834=LINE('',#21796,#5238);
#3835=LINE('',#21801,#5239);
#3836=LINE('',#21803,#5240);
#3837=LINE('',#21805,#5241);
#3838=LINE('',#21806,#5242);
#3839=LINE('',#21809,#5243);
#3840=LINE('',#21811,#5244);
#3841=LINE('',#21812,#5245);
#3842=LINE('',#21815,#5246);
#3843=LINE('',#21817,#5247);
#3844=LINE('',#21818,#5248);
#3845=LINE('',#21820,#5249);
#3846=LINE('',#21821,#5250);
#3847=LINE('',#21828,#5251);
#3848=LINE('',#21834,#5252);
#3849=LINE('',#21842,#5253);
#3850=LINE('',#21848,#5254);
#3851=LINE('',#21856,#5255);
#3852=LINE('',#21862,#5256);
#3853=LINE('',#21868,#5257);
#3854=LINE('',#21874,#5258);
#3855=LINE('',#21880,#5259);
#3856=LINE('',#21886,#5260);
#3857=LINE('',#21892,#5261);
#3858=LINE('',#21898,#5262);
#3859=LINE('',#21904,#5263);
#3860=LINE('',#21910,#5264);
#3861=LINE('',#21916,#5265);
#3862=LINE('',#21922,#5266);
#3863=LINE('',#21928,#5267);
#3864=LINE('',#21934,#5268);
#3865=LINE('',#21942,#5269);
#3866=LINE('',#21948,#5270);
#3867=LINE('',#21954,#5271);
#3868=LINE('',#21960,#5272);
#3869=LINE('',#21966,#5273);
#3870=LINE('',#21972,#5274);
#3871=LINE('',#21981,#5275);
#3872=LINE('',#21983,#5276);
#3873=LINE('',#21985,#5277);
#3874=LINE('',#21987,#5278);
#3875=LINE('',#21991,#5279);
#3876=LINE('',#21995,#5280);
#3877=LINE('',#22000,#5281);
#3878=LINE('',#22002,#5282);
#3879=LINE('',#22006,#5283);
#3880=LINE('',#22010,#5284);
#3881=LINE('',#22014,#5285);
#3882=LINE('',#22015,#5286);
#3883=LINE('',#22017,#5287);
#3884=LINE('',#22018,#5288);
#3885=LINE('',#22020,#5289);
#3886=LINE('',#22022,#5290);
#3887=LINE('',#22024,#5291);
#3888=LINE('',#22026,#5292);
#3889=LINE('',#22028,#5293);
#3890=LINE('',#22030,#5294);
#3891=LINE('',#22032,#5295);
#3892=LINE('',#22037,#5296);
#3893=LINE('',#22041,#5297);
#3894=LINE('',#22045,#5298);
#3895=LINE('',#22049,#5299);
#3896=LINE('',#22051,#5300);
#3897=LINE('',#22052,#5301);
#3898=LINE('',#22056,#5302);
#3899=LINE('',#22058,#5303);
#3900=LINE('',#22060,#5304);
#3901=LINE('',#22064,#5305);
#3902=LINE('',#22068,#5306);
#3903=LINE('',#22071,#5307);
#3904=LINE('',#22073,#5308);
#3905=LINE('',#22074,#5309);
#3906=LINE('',#22076,#5310);
#3907=LINE('',#22078,#5311);
#3908=LINE('',#22080,#5312);
#3909=LINE('',#22082,#5313);
#3910=LINE('',#22084,#5314);
#3911=LINE('',#22086,#5315);
#3912=LINE('',#22088,#5316);
#3913=LINE('',#22093,#5317);
#3914=LINE('',#22097,#5318);
#3915=LINE('',#22101,#5319);
#3916=LINE('',#22105,#5320);
#3917=LINE('',#22107,#5321);
#3918=LINE('',#22108,#5322);
#3919=LINE('',#22112,#5323);
#3920=LINE('',#22114,#5324);
#3921=LINE('',#22116,#5325);
#3922=LINE('',#22120,#5326);
#3923=LINE('',#22124,#5327);
#3924=LINE('',#22127,#5328);
#3925=LINE('',#22129,#5329);
#3926=LINE('',#22130,#5330);
#3927=LINE('',#22132,#5331);
#3928=LINE('',#22134,#5332);
#3929=LINE('',#22136,#5333);
#3930=LINE('',#22138,#5334);
#3931=LINE('',#22140,#5335);
#3932=LINE('',#22142,#5336);
#3933=LINE('',#22144,#5337);
#3934=LINE('',#22150,#5338);
#3935=LINE('',#22157,#5339);
#3936=LINE('',#22160,#5340);
#3937=LINE('',#22165,#5341);
#3938=LINE('',#22169,#5342);
#3939=LINE('',#22171,#5343);
#3940=LINE('',#22172,#5344);
#3941=LINE('',#22175,#5345);
#3942=LINE('',#22177,#5346);
#3943=LINE('',#22178,#5347);
#3944=LINE('',#22181,#5348);
#3945=LINE('',#22183,#5349);
#3946=LINE('',#22184,#5350);
#3947=LINE('',#22186,#5351);
#3948=LINE('',#22187,#5352);
#3949=LINE('',#22194,#5353);
#3950=LINE('',#22199,#5354);
#3951=LINE('',#22201,#5355);
#3952=LINE('',#22203,#5356);
#3953=LINE('',#22207,#5357);
#3954=LINE('',#22208,#5358);
#3955=LINE('',#22212,#5359);
#3956=LINE('',#22214,#5360);
#3957=LINE('',#22216,#5361);
#3958=LINE('',#22220,#5362);
#3959=LINE('',#22221,#5363);
#3960=LINE('',#22223,#5364);
#3961=LINE('',#22224,#5365);
#3962=LINE('',#22226,#5366);
#3963=LINE('',#22228,#5367);
#3964=LINE('',#22230,#5368);
#3965=LINE('',#22232,#5369);
#3966=LINE('',#22238,#5370);
#3967=LINE('',#22245,#5371);
#3968=LINE('',#22248,#5372);
#3969=LINE('',#22254,#5373);
#3970=LINE('',#22257,#5374);
#3971=LINE('',#22259,#5375);
#3972=LINE('',#22260,#5376);
#3973=LINE('',#22263,#5377);
#3974=LINE('',#22265,#5378);
#3975=LINE('',#22266,#5379);
#3976=LINE('',#22269,#5380);
#3977=LINE('',#22271,#5381);
#3978=LINE('',#22272,#5382);
#3979=LINE('',#22274,#5383);
#3980=LINE('',#22275,#5384);
#3981=LINE('',#22282,#5385);
#3982=LINE('',#22287,#5386);
#3983=LINE('',#22289,#5387);
#3984=LINE('',#22291,#5388);
#3985=LINE('',#22295,#5389);
#3986=LINE('',#22296,#5390);
#3987=LINE('',#22300,#5391);
#3988=LINE('',#22302,#5392);
#3989=LINE('',#22304,#5393);
#3990=LINE('',#22308,#5394);
#3991=LINE('',#22309,#5395);
#3992=LINE('',#22311,#5396);
#3993=LINE('',#22312,#5397);
#3994=LINE('',#22314,#5398);
#3995=LINE('',#22316,#5399);
#3996=LINE('',#22318,#5400);
#3997=LINE('',#22320,#5401);
#3998=LINE('',#22327,#5402);
#3999=LINE('',#22330,#5403);
#4000=LINE('',#22336,#5404);
#4001=LINE('',#22339,#5405);
#4002=LINE('',#22345,#5406);
#4003=LINE('',#22348,#5407);
#4004=LINE('',#22354,#5408);
#4005=LINE('',#22357,#5409);
#4006=LINE('',#22360,#5410);
#4007=LINE('',#22362,#5411);
#4008=LINE('',#22363,#5412);
#4009=LINE('',#22366,#5413);
#4010=LINE('',#22368,#5414);
#4011=LINE('',#22369,#5415);
#4012=LINE('',#22373,#5416);
#4013=LINE('',#22377,#5417);
#4014=LINE('',#22381,#5418);
#4015=LINE('',#22385,#5419);
#4016=LINE('',#22387,#5420);
#4017=LINE('',#22388,#5421);
#4018=LINE('',#22391,#5422);
#4019=LINE('',#22393,#5423);
#4020=LINE('',#22395,#5424);
#4021=LINE('',#22399,#5425);
#4022=LINE('',#22402,#5426);
#4023=LINE('',#22404,#5427);
#4024=LINE('',#22406,#5428);
#4025=LINE('',#22407,#5429);
#4026=LINE('',#22408,#5430);
#4027=LINE('',#22409,#5431);
#4028=LINE('',#22410,#5432);
#4029=LINE('',#22412,#5433);
#4030=LINE('',#22414,#5434);
#4031=LINE('',#22416,#5435);
#4032=LINE('',#22418,#5436);
#4033=LINE('',#22420,#5437);
#4034=LINE('',#22422,#5438);
#4035=LINE('',#22423,#5439);
#4036=LINE('',#22424,#5440);
#4037=LINE('',#22426,#5441);
#4038=LINE('',#22427,#5442);
#4039=LINE('',#22431,#5443);
#4040=LINE('',#22433,#5444);
#4041=LINE('',#22442,#5445);
#4042=LINE('',#22447,#5446);
#4043=LINE('',#22449,#5447);
#4044=LINE('',#22451,#5448);
#4045=LINE('',#22455,#5449);
#4046=LINE('',#22456,#5450);
#4047=LINE('',#22460,#5451);
#4048=LINE('',#22462,#5452);
#4049=LINE('',#22464,#5453);
#4050=LINE('',#22468,#5454);
#4051=LINE('',#22469,#5455);
#4052=LINE('',#22471,#5456);
#4053=LINE('',#22472,#5457);
#4054=LINE('',#22474,#5458);
#4055=LINE('',#22476,#5459);
#4056=LINE('',#22478,#5460);
#4057=LINE('',#22480,#5461);
#4058=LINE('',#22486,#5462);
#4059=LINE('',#22491,#5463);
#4060=LINE('',#22493,#5464);
#4061=LINE('',#22495,#5465);
#4062=LINE('',#22499,#5466);
#4063=LINE('',#22500,#5467);
#4064=LINE('',#22504,#5468);
#4065=LINE('',#22506,#5469);
#4066=LINE('',#22508,#5470);
#4067=LINE('',#22512,#5471);
#4068=LINE('',#22513,#5472);
#4069=LINE('',#22515,#5473);
#4070=LINE('',#22516,#5474);
#4071=LINE('',#22518,#5475);
#4072=LINE('',#22520,#5476);
#4073=LINE('',#22522,#5477);
#4074=LINE('',#22524,#5478);
#4075=LINE('',#22530,#5479);
#4076=LINE('',#22532,#5480);
#4077=LINE('',#22534,#5481);
#4078=LINE('',#22535,#5482);
#4079=LINE('',#22538,#5483);
#4080=LINE('',#22540,#5484);
#4081=LINE('',#22541,#5485);
#4082=LINE('',#22546,#5486);
#4083=LINE('',#22550,#5487);
#4084=LINE('',#22552,#5488);
#4085=LINE('',#22553,#5489);
#4086=LINE('',#22556,#5490);
#4087=LINE('',#22558,#5491);
#4088=LINE('',#22559,#5492);
#4089=LINE('',#22562,#5493);
#4090=LINE('',#22564,#5494);
#4091=LINE('',#22565,#5495);
#4092=LINE('',#22570,#5496);
#4093=LINE('',#22574,#5497);
#4094=LINE('',#22576,#5498);
#4095=LINE('',#22577,#5499);
#4096=LINE('',#22580,#5500);
#4097=LINE('',#22582,#5501);
#4098=LINE('',#22583,#5502);
#4099=LINE('',#22586,#5503);
#4100=LINE('',#22588,#5504);
#4101=LINE('',#22589,#5505);
#4102=LINE('',#22592,#5506);
#4103=LINE('',#22594,#5507);
#4104=LINE('',#22595,#5508);
#4105=LINE('',#22597,#5509);
#4106=LINE('',#22598,#5510);
#4107=LINE('',#22605,#5511);
#4108=LINE('',#22612,#5512);
#4109=LINE('',#22615,#5513);
#4110=LINE('',#22620,#5514);
#4111=LINE('',#22624,#5515);
#4112=LINE('',#22626,#5516);
#4113=LINE('',#22628,#5517);
#4114=LINE('',#22629,#5518);
#4115=LINE('',#22632,#5519);
#4116=LINE('',#22634,#5520);
#4117=LINE('',#22636,#5521);
#4118=LINE('',#22637,#5522);
#4119=LINE('',#22639,#5523);
#4120=LINE('',#22641,#5524);
#4121=LINE('',#22643,#5525);
#4122=LINE('',#22649,#5526);
#4123=LINE('',#22656,#5527);
#4124=LINE('',#22659,#5528);
#4125=LINE('',#22665,#5529);
#4126=LINE('',#22668,#5530);
#4127=LINE('',#22670,#5531);
#4128=LINE('',#22672,#5532);
#4129=LINE('',#22673,#5533);
#4130=LINE('',#22676,#5534);
#4131=LINE('',#22678,#5535);
#4132=LINE('',#22680,#5536);
#4133=LINE('',#22681,#5537);
#4134=LINE('',#22683,#5538);
#4135=LINE('',#22685,#5539);
#4136=LINE('',#22687,#5540);
#4137=LINE('',#22707,#5541);
#4138=LINE('',#22710,#5542);
#4139=LINE('',#22714,#5543);
#4140=LINE('',#22722,#5544);
#4141=LINE('',#22727,#5545);
#4142=LINE('',#22735,#5546);
#4143=LINE('',#22737,#5547);
#4144=LINE('',#22739,#5548);
#4145=LINE('',#22750,#5549);
#4146=LINE('',#22751,#5550);
#4147=LINE('',#22762,#5551);
#4148=LINE('',#22763,#5552);
#4149=LINE('',#22774,#5553);
#4150=LINE('',#22775,#5554);
#4151=LINE('',#22786,#5555);
#4152=LINE('',#22787,#5556);
#4153=LINE('',#22796,#5557);
#4154=LINE('',#22820,#5558);
#4155=LINE('',#22825,#5559);
#4156=LINE('',#22833,#5560);
#4157=LINE('',#22835,#5561);
#4158=LINE('',#22837,#5562);
#4159=LINE('',#22848,#5563);
#4160=LINE('',#22849,#5564);
#4161=LINE('',#22860,#5565);
#4162=LINE('',#22861,#5566);
#4163=LINE('',#22872,#5567);
#4164=LINE('',#22873,#5568);
#4165=LINE('',#22884,#5569);
#4166=LINE('',#22885,#5570);
#4167=LINE('',#22894,#5571);
#4168=LINE('',#22918,#5572);
#4169=LINE('',#22926,#5573);
#4170=LINE('',#22932,#5574);
#4171=LINE('',#22935,#5575);
#4172=LINE('',#22939,#5576);
#4173=LINE('',#22949,#5577);
#4174=LINE('',#22967,#5578);
#4175=LINE('',#22982,#5579);
#4176=LINE('',#23003,#5580);
#4177=LINE('',#23021,#5581);
#4178=LINE('',#23074,#5582);
#4179=LINE('',#23097,#5583);
#4180=LINE('',#23143,#5584);
#4181=LINE('',#23189,#5585);
#4182=LINE('',#23235,#5586);
#4183=LINE('',#23281,#5587);
#4184=LINE('',#23327,#5588);
#4185=LINE('',#23373,#5589);
#4186=LINE('',#23419,#5590);
#4187=LINE('',#23465,#5591);
#4188=LINE('',#23511,#5592);
#4189=LINE('',#23557,#5593);
#4190=LINE('',#23603,#5594);
#4191=LINE('',#23649,#5595);
#4192=LINE('',#23695,#5596);
#4193=LINE('',#23741,#5597);
#4194=LINE('',#23787,#5598);
#4195=LINE('',#23833,#5599);
#4196=LINE('',#23879,#5600);
#4197=LINE('',#23925,#5601);
#4198=LINE('',#23971,#5602);
#4199=LINE('',#24017,#5603);
#4200=LINE('',#24063,#5604);
#4201=LINE('',#24102,#5605);
#4202=LINE('',#24554,#5606);
#4203=LINE('',#24586,#5607);
#4204=LINE('',#24662,#5608);
#4205=LINE('',#24738,#5609);
#4206=LINE('',#24814,#5610);
#4207=LINE('',#24890,#5611);
#4208=LINE('',#24966,#5612);
#4209=LINE('',#25044,#5613);
#4210=LINE('',#25120,#5614);
#4211=LINE('',#25196,#5615);
#4212=LINE('',#25274,#5616);
#4213=LINE('',#25350,#5617);
#4214=LINE('',#25426,#5618);
#4215=LINE('',#25502,#5619);
#4216=LINE('',#25578,#5620);
#4217=LINE('',#25654,#5621);
#4218=LINE('',#25732,#5622);
#4219=LINE('',#25808,#5623);
#4220=LINE('',#25886,#5624);
#4221=LINE('',#25962,#5625);
#4222=LINE('',#26038,#5626);
#4223=LINE('',#26133,#5627);
#4224=LINE('',#26307,#5628);
#4225=LINE('',#26564,#5629);
#4226=LINE('',#26566,#5630);
#4227=LINE('',#26567,#5631);
#4228=LINE('',#29143,#5632);
#4229=LINE('',#29186,#5633);
#4230=LINE('',#29232,#5634);
#4231=LINE('',#29278,#5635);
#4232=LINE('',#29324,#5636);
#4233=LINE('',#29365,#5637);
#4234=LINE('',#29379,#5638);
#4235=LINE('',#29457,#5639);
#4236=LINE('',#29533,#5640);
#4237=LINE('',#29609,#5641);
#4238=LINE('',#29685,#5642);
#4239=LINE('',#29733,#5643);
#4240=LINE('',#29739,#5644);
#4241=LINE('',#29743,#5645);
#4242=LINE('',#29854,#5646);
#4243=LINE('',#29860,#5647);
#4244=LINE('',#29866,#5648);
#4245=LINE('',#29871,#5649);
#4246=LINE('',#29884,#5650);
#4247=LINE('',#29890,#5651);
#4248=LINE('',#29895,#5652);
#4249=LINE('',#29901,#5653);
#4250=LINE('',#29905,#5654);
#4251=LINE('',#29909,#5655);
#4252=LINE('',#29913,#5656);
#4253=LINE('',#29955,#5657);
#4254=LINE('',#29959,#5658);
#4255=LINE('',#29963,#5659);
#4256=LINE('',#29967,#5660);
#4257=LINE('',#30007,#5661);
#4258=LINE('',#30023,#5662);
#4259=LINE('',#30039,#5663);
#4260=LINE('',#30675,#5664);
#4261=LINE('',#30681,#5665);
#4262=LINE('',#30709,#5666);
#4263=LINE('',#30711,#5667);
#4264=LINE('',#30713,#5668);
#4265=LINE('',#30714,#5669);
#4266=LINE('',#30717,#5670);
#4267=LINE('',#30719,#5671);
#4268=LINE('',#30720,#5672);
#4269=LINE('',#30723,#5673);
#4270=LINE('',#30725,#5674);
#4271=LINE('',#30726,#5675);
#4272=LINE('',#30728,#5676);
#4273=LINE('',#30729,#5677);
#4274=LINE('',#30736,#5678);
#4275=LINE('',#30741,#5679);
#4276=LINE('',#30743,#5680);
#4277=LINE('',#30745,#5681);
#4278=LINE('',#30747,#5682);
#4279=LINE('',#30750,#5683);
#4280=LINE('',#30754,#5684);
#4281=LINE('',#30756,#5685);
#4282=LINE('',#30760,#5686);
#4283=LINE('',#30762,#5687);
#4284=LINE('',#30763,#5688);
#4285=LINE('',#30765,#5689);
#4286=LINE('',#30766,#5690);
#4287=LINE('',#30768,#5691);
#4288=LINE('',#30770,#5692);
#4289=LINE('',#30772,#5693);
#4290=LINE('',#30774,#5694);
#4291=LINE('',#30780,#5695);
#4292=LINE('',#30785,#5696);
#4293=LINE('',#30787,#5697);
#4294=LINE('',#30791,#5698);
#4295=LINE('',#30793,#5699);
#4296=LINE('',#30794,#5700);
#4297=LINE('',#30798,#5701);
#4298=LINE('',#30800,#5702);
#4299=LINE('',#30802,#5703);
#4300=LINE('',#30804,#5704);
#4301=LINE('',#30807,#5705);
#4302=LINE('',#30809,#5706);
#4303=LINE('',#30810,#5707);
#4304=LINE('',#30812,#5708);
#4305=LINE('',#30814,#5709);
#4306=LINE('',#30816,#5710);
#4307=LINE('',#30818,#5711);
#4308=LINE('',#30824,#5712);
#4309=LINE('',#30830,#5713);
#4310=LINE('',#30836,#5714);
#4311=LINE('',#30842,#5715);
#4312=LINE('',#30848,#5716);
#4313=LINE('',#30853,#5717);
#4314=LINE('',#30855,#5718);
#4315=LINE('',#30857,#5719);
#4316=LINE('',#30859,#5720);
#4317=LINE('',#30861,#5721);
#4318=LINE('',#30863,#5722);
#4319=LINE('',#30865,#5723);
#4320=LINE('',#30866,#5724);
#4321=LINE('',#30870,#5725);
#4322=LINE('',#30872,#5726);
#4323=LINE('',#30874,#5727);
#4324=LINE('',#30876,#5728);
#4325=LINE('',#30878,#5729);
#4326=LINE('',#30880,#5730);
#4327=LINE('',#30882,#5731);
#4328=LINE('',#30883,#5732);
#4329=LINE('',#30885,#5733);
#4330=LINE('',#30886,#5734);
#4331=LINE('',#30888,#5735);
#4332=LINE('',#30890,#5736);
#4333=LINE('',#30892,#5737);
#4334=LINE('',#30894,#5738);
#4335=LINE('',#30896,#5739);
#4336=LINE('',#30898,#5740);
#4337=LINE('',#30903,#5741);
#4338=LINE('',#30905,#5742);
#4339=LINE('',#30907,#5743);
#4340=LINE('',#30908,#5744);
#4341=LINE('',#30911,#5745);
#4342=LINE('',#30913,#5746);
#4343=LINE('',#30914,#5747);
#4344=LINE('',#30917,#5748);
#4345=LINE('',#30919,#5749);
#4346=LINE('',#30920,#5750);
#4347=LINE('',#30922,#5751);
#4348=LINE('',#30923,#5752);
#4349=LINE('',#30929,#5753);
#4350=LINE('',#30931,#5754);
#4351=LINE('',#30933,#5755);
#4352=LINE('',#30934,#5756);
#4353=LINE('',#30937,#5757);
#4354=LINE('',#30939,#5758);
#4355=LINE('',#30940,#5759);
#4356=LINE('',#30943,#5760);
#4357=LINE('',#30945,#5761);
#4358=LINE('',#30946,#5762);
#4359=LINE('',#30948,#5763);
#4360=LINE('',#30949,#5764);
#4361=LINE('',#30955,#5765);
#4362=LINE('',#30957,#5766);
#4363=LINE('',#30959,#5767);
#4364=LINE('',#30960,#5768);
#4365=LINE('',#30963,#5769);
#4366=LINE('',#30965,#5770);
#4367=LINE('',#30966,#5771);
#4368=LINE('',#30969,#5772);
#4369=LINE('',#30971,#5773);
#4370=LINE('',#30972,#5774);
#4371=LINE('',#30975,#5775);
#4372=LINE('',#30977,#5776);
#4373=LINE('',#30978,#5777);
#4374=LINE('',#30981,#5778);
#4375=LINE('',#30983,#5779);
#4376=LINE('',#30984,#5780);
#4377=LINE('',#30986,#5781);
#4378=LINE('',#30987,#5782);
#4379=LINE('',#30994,#5783);
#4380=LINE('',#31000,#5784);
#4381=LINE('',#31006,#5785);
#4382=LINE('',#31011,#5786);
#4383=LINE('',#31013,#5787);
#4384=LINE('',#31015,#5788);
#4385=LINE('',#31016,#5789);
#4386=LINE('',#31020,#5790);
#4387=LINE('',#31022,#5791);
#4388=LINE('',#31024,#5792);
#4389=LINE('',#31025,#5793);
#4390=LINE('',#31027,#5794);
#4391=LINE('',#31028,#5795);
#4392=LINE('',#31030,#5796);
#4393=LINE('',#31032,#5797);
#4394=LINE('',#31038,#5798);
#4395=LINE('',#31044,#5799);
#4396=LINE('',#31050,#5800);
#4397=LINE('',#31055,#5801);
#4398=LINE('',#31057,#5802);
#4399=LINE('',#31059,#5803);
#4400=LINE('',#31060,#5804);
#4401=LINE('',#31064,#5805);
#4402=LINE('',#31066,#5806);
#4403=LINE('',#31068,#5807);
#4404=LINE('',#31069,#5808);
#4405=LINE('',#31071,#5809);
#4406=LINE('',#31072,#5810);
#4407=LINE('',#31074,#5811);
#4408=LINE('',#31076,#5812);
#4409=LINE('',#31082,#5813);
#4410=LINE('',#31088,#5814);
#4411=LINE('',#31094,#5815);
#4412=LINE('',#31099,#5816);
#4413=LINE('',#31101,#5817);
#4414=LINE('',#31103,#5818);
#4415=LINE('',#31104,#5819);
#4416=LINE('',#31108,#5820);
#4417=LINE('',#31110,#5821);
#4418=LINE('',#31112,#5822);
#4419=LINE('',#31113,#5823);
#4420=LINE('',#31115,#5824);
#4421=LINE('',#31116,#5825);
#4422=LINE('',#31118,#5826);
#4423=LINE('',#31120,#5827);
#4424=LINE('',#31126,#5828);
#4425=LINE('',#31132,#5829);
#4426=LINE('',#31138,#5830);
#4427=LINE('',#31143,#5831);
#4428=LINE('',#31145,#5832);
#4429=LINE('',#31147,#5833);
#4430=LINE('',#31148,#5834);
#4431=LINE('',#31152,#5835);
#4432=LINE('',#31154,#5836);
#4433=LINE('',#31156,#5837);
#4434=LINE('',#31157,#5838);
#4435=LINE('',#31159,#5839);
#4436=LINE('',#31160,#5840);
#4437=LINE('',#31162,#5841);
#4438=LINE('',#31164,#5842);
#4439=LINE('',#31169,#5843);
#4440=LINE('',#31171,#5844);
#4441=LINE('',#31173,#5845);
#4442=LINE('',#31174,#5846);
#4443=LINE('',#31177,#5847);
#4444=LINE('',#31179,#5848);
#4445=LINE('',#31180,#5849);
#4446=LINE('',#31183,#5850);
#4447=LINE('',#31185,#5851);
#4448=LINE('',#31186,#5852);
#4449=LINE('',#31188,#5853);
#4450=LINE('',#31189,#5854);
#4451=LINE('',#31195,#5855);
#4452=LINE('',#31197,#5856);
#4453=LINE('',#31199,#5857);
#4454=LINE('',#31200,#5858);
#4455=LINE('',#31203,#5859);
#4456=LINE('',#31205,#5860);
#4457=LINE('',#31206,#5861);
#4458=LINE('',#31209,#5862);
#4459=LINE('',#31211,#5863);
#4460=LINE('',#31212,#5864);
#4461=LINE('',#31214,#5865);
#4462=LINE('',#31215,#5866);
#4463=LINE('',#31221,#5867);
#4464=LINE('',#31223,#5868);
#4465=LINE('',#31225,#5869);
#4466=LINE('',#31226,#5870);
#4467=LINE('',#31229,#5871);
#4468=LINE('',#31231,#5872);
#4469=LINE('',#31232,#5873);
#4470=LINE('',#31235,#5874);
#4471=LINE('',#31237,#5875);
#4472=LINE('',#31238,#5876);
#4473=LINE('',#31240,#5877);
#4474=LINE('',#31241,#5878);
#4475=LINE('',#31247,#5879);
#4476=LINE('',#31249,#5880);
#4477=LINE('',#31251,#5881);
#4478=LINE('',#31252,#5882);
#4479=LINE('',#31255,#5883);
#4480=LINE('',#31257,#5884);
#4481=LINE('',#31258,#5885);
#4482=LINE('',#31261,#5886);
#4483=LINE('',#31263,#5887);
#4484=LINE('',#31264,#5888);
#4485=LINE('',#31266,#5889);
#4486=LINE('',#31267,#5890);
#4487=LINE('',#31273,#5891);
#4488=LINE('',#31275,#5892);
#4489=LINE('',#31277,#5893);
#4490=LINE('',#31278,#5894);
#4491=LINE('',#31281,#5895);
#4492=LINE('',#31283,#5896);
#4493=LINE('',#31284,#5897);
#4494=LINE('',#31287,#5898);
#4495=LINE('',#31289,#5899);
#4496=LINE('',#31290,#5900);
#4497=LINE('',#31292,#5901);
#4498=LINE('',#31293,#5902);
#4499=LINE('',#31300,#5903);
#4500=LINE('',#31306,#5904);
#4501=LINE('',#31312,#5905);
#4502=LINE('',#31318,#5906);
#4503=LINE('',#31323,#5907);
#4504=LINE('',#31325,#5908);
#4505=LINE('',#31327,#5909);
#4506=LINE('',#31328,#5910);
#4507=LINE('',#31332,#5911);
#4508=LINE('',#31334,#5912);
#4509=LINE('',#31336,#5913);
#4510=LINE('',#31337,#5914);
#4511=LINE('',#31339,#5915);
#4512=LINE('',#31340,#5916);
#4513=LINE('',#31342,#5917);
#4514=LINE('',#31344,#5918);
#4515=LINE('',#31350,#5919);
#4516=LINE('',#31356,#5920);
#4517=LINE('',#31362,#5921);
#4518=LINE('',#31368,#5922);
#4519=LINE('',#31374,#5923);
#4520=LINE('',#31380,#5924);
#4521=LINE('',#31385,#5925);
#4522=LINE('',#31387,#5926);
#4523=LINE('',#31389,#5927);
#4524=LINE('',#31390,#5928);
#4525=LINE('',#31393,#5929);
#4526=LINE('',#31395,#5930);
#4527=LINE('',#31396,#5931);
#4528=LINE('',#31399,#5932);
#4529=LINE('',#31401,#5933);
#4530=LINE('',#31402,#5934);
#4531=LINE('',#31404,#5935);
#4532=LINE('',#31405,#5936);
#4533=LINE('',#31411,#5937);
#4534=LINE('',#31413,#5938);
#4535=LINE('',#31415,#5939);
#4536=LINE('',#31416,#5940);
#4537=LINE('',#31419,#5941);
#4538=LINE('',#31421,#5942);
#4539=LINE('',#31422,#5943);
#4540=LINE('',#31425,#5944);
#4541=LINE('',#31427,#5945);
#4542=LINE('',#31428,#5946);
#4543=LINE('',#31431,#5947);
#4544=LINE('',#31433,#5948);
#4545=LINE('',#31434,#5949);
#4546=LINE('',#31437,#5950);
#4547=LINE('',#31439,#5951);
#4548=LINE('',#31440,#5952);
#4549=LINE('',#31443,#5953);
#4550=LINE('',#31445,#5954);
#4551=LINE('',#31446,#5955);
#4552=LINE('',#31448,#5956);
#4553=LINE('',#31449,#5957);
#4554=LINE('',#31455,#5958);
#4555=LINE('',#31457,#5959);
#4556=LINE('',#31459,#5960);
#4557=LINE('',#31460,#5961);
#4558=LINE('',#31463,#5962);
#4559=LINE('',#31465,#5963);
#4560=LINE('',#31466,#5964);
#4561=LINE('',#31469,#5965);
#4562=LINE('',#31471,#5966);
#4563=LINE('',#31472,#5967);
#4564=LINE('',#31475,#5968);
#4565=LINE('',#31477,#5969);
#4566=LINE('',#31478,#5970);
#4567=LINE('',#31481,#5971);
#4568=LINE('',#31483,#5972);
#4569=LINE('',#31484,#5973);
#4570=LINE('',#31487,#5974);
#4571=LINE('',#31489,#5975);
#4572=LINE('',#31490,#5976);
#4573=LINE('',#31492,#5977);
#4574=LINE('',#31493,#5978);
#4575=LINE('',#31499,#5979);
#4576=LINE('',#31501,#5980);
#4577=LINE('',#31503,#5981);
#4578=LINE('',#31504,#5982);
#4579=LINE('',#31507,#5983);
#4580=LINE('',#31509,#5984);
#4581=LINE('',#31510,#5985);
#4582=LINE('',#31513,#5986);
#4583=LINE('',#31515,#5987);
#4584=LINE('',#31516,#5988);
#4585=LINE('',#31519,#5989);
#4586=LINE('',#31521,#5990);
#4587=LINE('',#31522,#5991);
#4588=LINE('',#31525,#5992);
#4589=LINE('',#31527,#5993);
#4590=LINE('',#31528,#5994);
#4591=LINE('',#31531,#5995);
#4592=LINE('',#31533,#5996);
#4593=LINE('',#31534,#5997);
#4594=LINE('',#31536,#5998);
#4595=LINE('',#31537,#5999);
#4596=LINE('',#31543,#6000);
#4597=LINE('',#31545,#6001);
#4598=LINE('',#31547,#6002);
#4599=LINE('',#31548,#6003);
#4600=LINE('',#31551,#6004);
#4601=LINE('',#31553,#6005);
#4602=LINE('',#31554,#6006);
#4603=LINE('',#31557,#6007);
#4604=LINE('',#31559,#6008);
#4605=LINE('',#31560,#6009);
#4606=LINE('',#31563,#6010);
#4607=LINE('',#31565,#6011);
#4608=LINE('',#31566,#6012);
#4609=LINE('',#31569,#6013);
#4610=LINE('',#31571,#6014);
#4611=LINE('',#31572,#6015);
#4612=LINE('',#31575,#6016);
#4613=LINE('',#31577,#6017);
#4614=LINE('',#31578,#6018);
#4615=LINE('',#31580,#6019);
#4616=LINE('',#31581,#6020);
#4617=LINE('',#31587,#6021);
#4618=LINE('',#31589,#6022);
#4619=LINE('',#31591,#6023);
#4620=LINE('',#31592,#6024);
#4621=LINE('',#31595,#6025);
#4622=LINE('',#31597,#6026);
#4623=LINE('',#31598,#6027);
#4624=LINE('',#31601,#6028);
#4625=LINE('',#31603,#6029);
#4626=LINE('',#31604,#6030);
#4627=LINE('',#31607,#6031);
#4628=LINE('',#31609,#6032);
#4629=LINE('',#31610,#6033);
#4630=LINE('',#31613,#6034);
#4631=LINE('',#31615,#6035);
#4632=LINE('',#31616,#6036);
#4633=LINE('',#31619,#6037);
#4634=LINE('',#31621,#6038);
#4635=LINE('',#31622,#6039);
#4636=LINE('',#31624,#6040);
#4637=LINE('',#31625,#6041);
#4638=LINE('',#31631,#6042);
#4639=LINE('',#31633,#6043);
#4640=LINE('',#31635,#6044);
#4641=LINE('',#31636,#6045);
#4642=LINE('',#31639,#6046);
#4643=LINE('',#31641,#6047);
#4644=LINE('',#31642,#6048);
#4645=LINE('',#31645,#6049);
#4646=LINE('',#31647,#6050);
#4647=LINE('',#31648,#6051);
#4648=LINE('',#31651,#6052);
#4649=LINE('',#31653,#6053);
#4650=LINE('',#31654,#6054);
#4651=LINE('',#31657,#6055);
#4652=LINE('',#31659,#6056);
#4653=LINE('',#31660,#6057);
#4654=LINE('',#31663,#6058);
#4655=LINE('',#31665,#6059);
#4656=LINE('',#31666,#6060);
#4657=LINE('',#31668,#6061);
#4658=LINE('',#31669,#6062);
#4659=LINE('',#31675,#6063);
#4660=LINE('',#31677,#6064);
#4661=LINE('',#31679,#6065);
#4662=LINE('',#31680,#6066);
#4663=LINE('',#31683,#6067);
#4664=LINE('',#31685,#6068);
#4665=LINE('',#31686,#6069);
#4666=LINE('',#31689,#6070);
#4667=LINE('',#31691,#6071);
#4668=LINE('',#31692,#6072);
#4669=LINE('',#31695,#6073);
#4670=LINE('',#31697,#6074);
#4671=LINE('',#31698,#6075);
#4672=LINE('',#31701,#6076);
#4673=LINE('',#31703,#6077);
#4674=LINE('',#31704,#6078);
#4675=LINE('',#31707,#6079);
#4676=LINE('',#31709,#6080);
#4677=LINE('',#31710,#6081);
#4678=LINE('',#31712,#6082);
#4679=LINE('',#31713,#6083);
#4680=LINE('',#31719,#6084);
#4681=LINE('',#31721,#6085);
#4682=LINE('',#31723,#6086);
#4683=LINE('',#31724,#6087);
#4684=LINE('',#31727,#6088);
#4685=LINE('',#31729,#6089);
#4686=LINE('',#31730,#6090);
#4687=LINE('',#31733,#6091);
#4688=LINE('',#31735,#6092);
#4689=LINE('',#31736,#6093);
#4690=LINE('',#31739,#6094);
#4691=LINE('',#31741,#6095);
#4692=LINE('',#31742,#6096);
#4693=LINE('',#31745,#6097);
#4694=LINE('',#31747,#6098);
#4695=LINE('',#31748,#6099);
#4696=LINE('',#31751,#6100);
#4697=LINE('',#31753,#6101);
#4698=LINE('',#31754,#6102);
#4699=LINE('',#31756,#6103);
#4700=LINE('',#31757,#6104);
#4701=LINE('',#31763,#6105);
#4702=LINE('',#31765,#6106);
#4703=LINE('',#31767,#6107);
#4704=LINE('',#31768,#6108);
#4705=LINE('',#31771,#6109);
#4706=LINE('',#31773,#6110);
#4707=LINE('',#31774,#6111);
#4708=LINE('',#31777,#6112);
#4709=LINE('',#31779,#6113);
#4710=LINE('',#31780,#6114);
#4711=LINE('',#31783,#6115);
#4712=LINE('',#31785,#6116);
#4713=LINE('',#31786,#6117);
#4714=LINE('',#31789,#6118);
#4715=LINE('',#31791,#6119);
#4716=LINE('',#31792,#6120);
#4717=LINE('',#31795,#6121);
#4718=LINE('',#31797,#6122);
#4719=LINE('',#31798,#6123);
#4720=LINE('',#31800,#6124);
#4721=LINE('',#31801,#6125);
#4722=LINE('',#31807,#6126);
#4723=LINE('',#31809,#6127);
#4724=LINE('',#31811,#6128);
#4725=LINE('',#31812,#6129);
#4726=LINE('',#31815,#6130);
#4727=LINE('',#31817,#6131);
#4728=LINE('',#31818,#6132);
#4729=LINE('',#31821,#6133);
#4730=LINE('',#31823,#6134);
#4731=LINE('',#31824,#6135);
#4732=LINE('',#31827,#6136);
#4733=LINE('',#31829,#6137);
#4734=LINE('',#31830,#6138);
#4735=LINE('',#31833,#6139);
#4736=LINE('',#31835,#6140);
#4737=LINE('',#31836,#6141);
#4738=LINE('',#31839,#6142);
#4739=LINE('',#31841,#6143);
#4740=LINE('',#31842,#6144);
#4741=LINE('',#31844,#6145);
#4742=LINE('',#31845,#6146);
#4743=LINE('',#31851,#6147);
#4744=LINE('',#31853,#6148);
#4745=LINE('',#31855,#6149);
#4746=LINE('',#31856,#6150);
#4747=LINE('',#31859,#6151);
#4748=LINE('',#31861,#6152);
#4749=LINE('',#31862,#6153);
#4750=LINE('',#31865,#6154);
#4751=LINE('',#31867,#6155);
#4752=LINE('',#31868,#6156);
#4753=LINE('',#31871,#6157);
#4754=LINE('',#31873,#6158);
#4755=LINE('',#31874,#6159);
#4756=LINE('',#31877,#6160);
#4757=LINE('',#31879,#6161);
#4758=LINE('',#31880,#6162);
#4759=LINE('',#31883,#6163);
#4760=LINE('',#31885,#6164);
#4761=LINE('',#31886,#6165);
#4762=LINE('',#31888,#6166);
#4763=LINE('',#31889,#6167);
#4764=LINE('',#31896,#6168);
#4765=LINE('',#31902,#6169);
#4766=LINE('',#31908,#6170);
#4767=LINE('',#31914,#6171);
#4768=LINE('',#31919,#6172);
#4769=LINE('',#31921,#6173);
#4770=LINE('',#31923,#6174);
#4771=LINE('',#31924,#6175);
#4772=LINE('',#31928,#6176);
#4773=LINE('',#31930,#6177);
#4774=LINE('',#31932,#6178);
#4775=LINE('',#31933,#6179);
#4776=LINE('',#31935,#6180);
#4777=LINE('',#31936,#6181);
#4778=LINE('',#31938,#6182);
#4779=LINE('',#31940,#6183);
#4780=LINE('',#31945,#6184);
#4781=LINE('',#31947,#6185);
#4782=LINE('',#31949,#6186);
#4783=LINE('',#31950,#6187);
#4784=LINE('',#31953,#6188);
#4785=LINE('',#31955,#6189);
#4786=LINE('',#31956,#6190);
#4787=LINE('',#31959,#6191);
#4788=LINE('',#31961,#6192);
#4789=LINE('',#31962,#6193);
#4790=LINE('',#31964,#6194);
#4791=LINE('',#31965,#6195);
#4792=LINE('',#31971,#6196);
#4793=LINE('',#31973,#6197);
#4794=LINE('',#31975,#6198);
#4795=LINE('',#31976,#6199);
#4796=LINE('',#31979,#6200);
#4797=LINE('',#31981,#6201);
#4798=LINE('',#31982,#6202);
#4799=LINE('',#31985,#6203);
#4800=LINE('',#31987,#6204);
#4801=LINE('',#31988,#6205);
#4802=LINE('',#31990,#6206);
#4803=LINE('',#31991,#6207);
#4804=LINE('',#31997,#6208);
#4805=LINE('',#31999,#6209);
#4806=LINE('',#32001,#6210);
#4807=LINE('',#32002,#6211);
#4808=LINE('',#32005,#6212);
#4809=LINE('',#32007,#6213);
#4810=LINE('',#32008,#6214);
#4811=LINE('',#32011,#6215);
#4812=LINE('',#32013,#6216);
#4813=LINE('',#32014,#6217);
#4814=LINE('',#32016,#6218);
#4815=LINE('',#32017,#6219);
#4816=LINE('',#32023,#6220);
#4817=LINE('',#32025,#6221);
#4818=LINE('',#32027,#6222);
#4819=LINE('',#32028,#6223);
#4820=LINE('',#32031,#6224);
#4821=LINE('',#32033,#6225);
#4822=LINE('',#32034,#6226);
#4823=LINE('',#32037,#6227);
#4824=LINE('',#32039,#6228);
#4825=LINE('',#32040,#6229);
#4826=LINE('',#32042,#6230);
#4827=LINE('',#32043,#6231);
#4828=LINE('',#32049,#6232);
#4829=LINE('',#32051,#6233);
#4830=LINE('',#32053,#6234);
#4831=LINE('',#32054,#6235);
#4832=LINE('',#32057,#6236);
#4833=LINE('',#32059,#6237);
#4834=LINE('',#32060,#6238);
#4835=LINE('',#32063,#6239);
#4836=LINE('',#32065,#6240);
#4837=LINE('',#32066,#6241);
#4838=LINE('',#32068,#6242);
#4839=LINE('',#32069,#6243);
#4840=LINE('',#32075,#6244);
#4841=LINE('',#32077,#6245);
#4842=LINE('',#32079,#6246);
#4843=LINE('',#32080,#6247);
#4844=LINE('',#32083,#6248);
#4845=LINE('',#32085,#6249);
#4846=LINE('',#32086,#6250);
#4847=LINE('',#32089,#6251);
#4848=LINE('',#32091,#6252);
#4849=LINE('',#32092,#6253);
#4850=LINE('',#32094,#6254);
#4851=LINE('',#32095,#6255);
#4852=LINE('',#32101,#6256);
#4853=LINE('',#32103,#6257);
#4854=LINE('',#32105,#6258);
#4855=LINE('',#32106,#6259);
#4856=LINE('',#32109,#6260);
#4857=LINE('',#32111,#6261);
#4858=LINE('',#32112,#6262);
#4859=LINE('',#32115,#6263);
#4860=LINE('',#32117,#6264);
#4861=LINE('',#32118,#6265);
#4862=LINE('',#32120,#6266);
#4863=LINE('',#32121,#6267);
#4864=LINE('',#32127,#6268);
#4865=LINE('',#32129,#6269);
#4866=LINE('',#32131,#6270);
#4867=LINE('',#32132,#6271);
#4868=LINE('',#32135,#6272);
#4869=LINE('',#32137,#6273);
#4870=LINE('',#32138,#6274);
#4871=LINE('',#32141,#6275);
#4872=LINE('',#32143,#6276);
#4873=LINE('',#32144,#6277);
#4874=LINE('',#32146,#6278);
#4875=LINE('',#32147,#6279);
#4876=LINE('',#32153,#6280);
#4877=LINE('',#32155,#6281);
#4878=LINE('',#32157,#6282);
#4879=LINE('',#32158,#6283);
#4880=LINE('',#32161,#6284);
#4881=LINE('',#32163,#6285);
#4882=LINE('',#32164,#6286);
#4883=LINE('',#32167,#6287);
#4884=LINE('',#32169,#6288);
#4885=LINE('',#32170,#6289);
#4886=LINE('',#32172,#6290);
#4887=LINE('',#32173,#6291);
#4888=LINE('',#32179,#6292);
#4889=LINE('',#32181,#6293);
#4890=LINE('',#32183,#6294);
#4891=LINE('',#32184,#6295);
#4892=LINE('',#32187,#6296);
#4893=LINE('',#32189,#6297);
#4894=LINE('',#32190,#6298);
#4895=LINE('',#32193,#6299);
#4896=LINE('',#32195,#6300);
#4897=LINE('',#32196,#6301);
#4898=LINE('',#32198,#6302);
#4899=LINE('',#32199,#6303);
#4900=LINE('',#32205,#6304);
#4901=LINE('',#32207,#6305);
#4902=LINE('',#32209,#6306);
#4903=LINE('',#32210,#6307);
#4904=LINE('',#32213,#6308);
#4905=LINE('',#32215,#6309);
#4906=LINE('',#32216,#6310);
#4907=LINE('',#32219,#6311);
#4908=LINE('',#32221,#6312);
#4909=LINE('',#32222,#6313);
#4910=LINE('',#32224,#6314);
#4911=LINE('',#32225,#6315);
#4912=LINE('',#32231,#6316);
#4913=LINE('',#32233,#6317);
#4914=LINE('',#32235,#6318);
#4915=LINE('',#32236,#6319);
#4916=LINE('',#32239,#6320);
#4917=LINE('',#32241,#6321);
#4918=LINE('',#32242,#6322);
#4919=LINE('',#32245,#6323);
#4920=LINE('',#32247,#6324);
#4921=LINE('',#32248,#6325);
#4922=LINE('',#32250,#6326);
#4923=LINE('',#32251,#6327);
#4924=LINE('',#32257,#6328);
#4925=LINE('',#32259,#6329);
#4926=LINE('',#32261,#6330);
#4927=LINE('',#32262,#6331);
#4928=LINE('',#32265,#6332);
#4929=LINE('',#32267,#6333);
#4930=LINE('',#32268,#6334);
#4931=LINE('',#32271,#6335);
#4932=LINE('',#32273,#6336);
#4933=LINE('',#32274,#6337);
#4934=LINE('',#32276,#6338);
#4935=LINE('',#32277,#6339);
#4936=LINE('',#32283,#6340);
#4937=LINE('',#32285,#6341);
#4938=LINE('',#32287,#6342);
#4939=LINE('',#32288,#6343);
#4940=LINE('',#32291,#6344);
#4941=LINE('',#32293,#6345);
#4942=LINE('',#32294,#6346);
#4943=LINE('',#32297,#6347);
#4944=LINE('',#32299,#6348);
#4945=LINE('',#32300,#6349);
#4946=LINE('',#32302,#6350);
#4947=LINE('',#32303,#6351);
#4948=LINE('',#32309,#6352);
#4949=LINE('',#32311,#6353);
#4950=LINE('',#32313,#6354);
#4951=LINE('',#32314,#6355);
#4952=LINE('',#32317,#6356);
#4953=LINE('',#32319,#6357);
#4954=LINE('',#32320,#6358);
#4955=LINE('',#32323,#6359);
#4956=LINE('',#32325,#6360);
#4957=LINE('',#32326,#6361);
#4958=LINE('',#32328,#6362);
#4959=LINE('',#32329,#6363);
#4960=LINE('',#32335,#6364);
#4961=LINE('',#32337,#6365);
#4962=LINE('',#32339,#6366);
#4963=LINE('',#32340,#6367);
#4964=LINE('',#32343,#6368);
#4965=LINE('',#32345,#6369);
#4966=LINE('',#32346,#6370);
#4967=LINE('',#32349,#6371);
#4968=LINE('',#32351,#6372);
#4969=LINE('',#32352,#6373);
#4970=LINE('',#32354,#6374);
#4971=LINE('',#32355,#6375);
#4972=LINE('',#32361,#6376);
#4973=LINE('',#32363,#6377);
#4974=LINE('',#32365,#6378);
#4975=LINE('',#32366,#6379);
#4976=LINE('',#32369,#6380);
#4977=LINE('',#32371,#6381);
#4978=LINE('',#32372,#6382);
#4979=LINE('',#32375,#6383);
#4980=LINE('',#32377,#6384);
#4981=LINE('',#32378,#6385);
#4982=LINE('',#32380,#6386);
#4983=LINE('',#32381,#6387);
#4984=LINE('',#32387,#6388);
#4985=LINE('',#32389,#6389);
#4986=LINE('',#32391,#6390);
#4987=LINE('',#32392,#6391);
#4988=LINE('',#32395,#6392);
#4989=LINE('',#32397,#6393);
#4990=LINE('',#32398,#6394);
#4991=LINE('',#32401,#6395);
#4992=LINE('',#32403,#6396);
#4993=LINE('',#32404,#6397);
#4994=LINE('',#32406,#6398);
#4995=LINE('',#32407,#6399);
#4996=LINE('',#32413,#6400);
#4997=LINE('',#32415,#6401);
#4998=LINE('',#32417,#6402);
#4999=LINE('',#32418,#6403);
#5000=LINE('',#32421,#6404);
#5001=LINE('',#32423,#6405);
#5002=LINE('',#32424,#6406);
#5003=LINE('',#32427,#6407);
#5004=LINE('',#32429,#6408);
#5005=LINE('',#32430,#6409);
#5006=LINE('',#32432,#6410);
#5007=LINE('',#32433,#6411);
#5008=LINE('',#32439,#6412);
#5009=LINE('',#32441,#6413);
#5010=LINE('',#32443,#6414);
#5011=LINE('',#32444,#6415);
#5012=LINE('',#32447,#6416);
#5013=LINE('',#32449,#6417);
#5014=LINE('',#32450,#6418);
#5015=LINE('',#32453,#6419);
#5016=LINE('',#32455,#6420);
#5017=LINE('',#32456,#6421);
#5018=LINE('',#32458,#6422);
#5019=LINE('',#32459,#6423);
#5020=LINE('',#32465,#6424);
#5021=LINE('',#32467,#6425);
#5022=LINE('',#32469,#6426);
#5023=LINE('',#32470,#6427);
#5024=LINE('',#32473,#6428);
#5025=LINE('',#32475,#6429);
#5026=LINE('',#32476,#6430);
#5027=LINE('',#32479,#6431);
#5028=LINE('',#32481,#6432);
#5029=LINE('',#32482,#6433);
#5030=LINE('',#32484,#6434);
#5031=LINE('',#32485,#6435);
#5032=LINE('',#32491,#6436);
#5033=LINE('',#32493,#6437);
#5034=LINE('',#32495,#6438);
#5035=LINE('',#32496,#6439);
#5036=LINE('',#32499,#6440);
#5037=LINE('',#32501,#6441);
#5038=LINE('',#32502,#6442);
#5039=LINE('',#32505,#6443);
#5040=LINE('',#32507,#6444);
#5041=LINE('',#32508,#6445);
#5042=LINE('',#32510,#6446);
#5043=LINE('',#32511,#6447);
#5044=LINE('',#32532,#6448);
#5045=LINE('',#32543,#6449);
#5046=LINE('',#32546,#6450);
#5047=LINE('',#32551,#6451);
#5048=LINE('',#32552,#6452);
#5049=LINE('',#32555,#6453);
#5050=LINE('',#32556,#6454);
#5051=LINE('',#32559,#6455);
#5052=LINE('',#32560,#6456);
#5053=LINE('',#32563,#6457);
#5054=LINE('',#32564,#6458);
#5055=LINE('',#32567,#6459);
#5056=LINE('',#32568,#6460);
#5057=LINE('',#32571,#6461);
#5058=LINE('',#32572,#6462);
#5059=LINE('',#32635,#6463);
#5060=LINE('',#32636,#6464);
#5061=LINE('',#32638,#6465);
#5062=LINE('',#32640,#6466);
#5063=LINE('',#32642,#6467);
#5064=LINE('',#32644,#6468);
#5065=LINE('',#32651,#6469);
#5066=LINE('',#32657,#6470);
#5067=LINE('',#32666,#6471);
#5068=LINE('',#32674,#6472);
#5069=LINE('',#32680,#6473);
#5070=LINE('',#32683,#6474);
#5071=LINE('',#32687,#6475);
#5072=LINE('',#32697,#6476);
#5073=LINE('',#32715,#6477);
#5074=LINE('',#32730,#6478);
#5075=LINE('',#32751,#6479);
#5076=LINE('',#32769,#6480);
#5077=VECTOR('',#17163,1000.);
#5078=VECTOR('',#17164,1000.);
#5079=VECTOR('',#17165,1000.);
#5080=VECTOR('',#17166,1000.);
#5081=VECTOR('',#17169,1000.);
#5082=VECTOR('',#17170,1000.);
#5083=VECTOR('',#17171,1000.);
#5084=VECTOR('',#17174,1000.);
#5085=VECTOR('',#17175,1000.);
#5086=VECTOR('',#17176,1000.);
#5087=VECTOR('',#17179,1000.);
#5088=VECTOR('',#17180,1000.);
#5089=VECTOR('',#17183,1000.);
#5090=VECTOR('',#17184,1000.);
#5091=VECTOR('',#17185,1000.);
#5092=VECTOR('',#17186,1000.);
#5093=VECTOR('',#17189,1000.);
#5094=VECTOR('',#17190,1000.);
#5095=VECTOR('',#17191,1000.);
#5096=VECTOR('',#17192,1000.);
#5097=VECTOR('',#17195,1000.);
#5098=VECTOR('',#17196,1000.);
#5099=VECTOR('',#17199,1000.);
#5100=VECTOR('',#17202,1000.);
#5101=VECTOR('',#17207,1000.);
#5102=VECTOR('',#17208,1000.);
#5103=VECTOR('',#17209,1000.);
#5104=VECTOR('',#17210,1000.);
#5105=VECTOR('',#17213,1000.);
#5106=VECTOR('',#17214,1000.);
#5107=VECTOR('',#17215,1000.);
#5108=VECTOR('',#17220,1000.);
#5109=VECTOR('',#17225,1000.);
#5110=VECTOR('',#17226,1000.);
#5111=VECTOR('',#17227,1000.);
#5112=VECTOR('',#17230,1000.);
#5113=VECTOR('',#17231,1000.);
#5114=VECTOR('',#17232,1000.);
#5115=VECTOR('',#17235,1000.);
#5116=VECTOR('',#17236,1000.);
#5117=VECTOR('',#17243,1000.);
#5118=VECTOR('',#17244,1000.);
#5119=VECTOR('',#17245,1000.);
#5120=VECTOR('',#17246,1000.);
#5121=VECTOR('',#17249,1000.);
#5122=VECTOR('',#17250,1000.);
#5123=VECTOR('',#17251,1000.);
#5124=VECTOR('',#17258,1000.);
#5125=VECTOR('',#17261,1000.);
#5126=VECTOR('',#17262,1000.);
#5127=VECTOR('',#17263,1000.);
#5128=VECTOR('',#17266,1000.);
#5129=VECTOR('',#17267,1000.);
#5130=VECTOR('',#17268,1000.);
#5131=VECTOR('',#17271,1000.);
#5132=VECTOR('',#17272,1000.);
#5133=VECTOR('',#17281,8.99999999999998);
#5134=VECTOR('',#17288,8.99999999999998);
#5135=VECTOR('',#17295,8.99999999999998);
#5136=VECTOR('',#17302,8.99999999999998);
#5137=VECTOR('',#17309,8.99999999999998);
#5138=VECTOR('',#17316,8.99999999999998);
#5139=VECTOR('',#17321,1000.);
#5140=VECTOR('',#17322,1000.);
#5141=VECTOR('',#17323,1000.);
#5142=VECTOR('',#17324,1000.);
#5143=VECTOR('',#17327,1000.);
#5144=VECTOR('',#17328,1000.);
#5145=VECTOR('',#17329,1000.);
#5146=VECTOR('',#17330,1000.);
#5147=VECTOR('',#17333,1000.);
#5148=VECTOR('',#17334,1000.);
#5149=VECTOR('',#17337,1000.);
#5150=VECTOR('',#17340,1000.);
#5151=VECTOR('',#17347,8.99999999999998);
#5152=VECTOR('',#17354,9.00000000000001);
#5153=VECTOR('',#17361,9.00000000000001);
#5154=VECTOR('',#17368,9.00000000000001);
#5155=VECTOR('',#17375,9.00000000000001);
#5156=VECTOR('',#17380,1000.);
#5157=VECTOR('',#17381,1000.);
#5158=VECTOR('',#17382,1000.);
#5159=VECTOR('',#17383,1000.);
#5160=VECTOR('',#17386,1000.);
#5161=VECTOR('',#17387,1000.);
#5162=VECTOR('',#17388,1000.);
#5163=VECTOR('',#17391,1000.);
#5164=VECTOR('',#17392,1000.);
#5165=VECTOR('',#17393,1000.);
#5166=VECTOR('',#17396,1000.);
#5167=VECTOR('',#17397,1000.);
#5168=VECTOR('',#17406,8.99999999999998);
#5169=VECTOR('',#17413,9.00000000000001);
#5170=VECTOR('',#17420,9.00000000000001);
#5171=VECTOR('',#17427,9.00000000000001);
#5172=VECTOR('',#17434,9.00000000000001);
#5173=VECTOR('',#17439,1000.);
#5174=VECTOR('',#17440,1000.);
#5175=VECTOR('',#17441,1000.);
#5176=VECTOR('',#17442,1000.);
#5177=VECTOR('',#17445,1000.);
#5178=VECTOR('',#17446,1000.);
#5179=VECTOR('',#17447,1000.);
#5180=VECTOR('',#17450,1000.);
#5181=VECTOR('',#17451,1000.);
#5182=VECTOR('',#17452,1000.);
#5183=VECTOR('',#17455,1000.);
#5184=VECTOR('',#17456,1000.);
#5185=VECTOR('',#17463,1000.);
#5186=VECTOR('',#17464,1000.);
#5187=VECTOR('',#17465,1000.);
#5188=VECTOR('',#17466,1000.);
#5189=VECTOR('',#17469,1000.);
#5190=VECTOR('',#17470,1000.);
#5191=VECTOR('',#17471,1000.);
#5192=VECTOR('',#17474,1000.);
#5193=VECTOR('',#17475,1000.);
#5194=VECTOR('',#17476,1000.);
#5195=VECTOR('',#17479,1000.);
#5196=VECTOR('',#17480,1000.);
#5197=VECTOR('',#17487,1000.);
#5198=VECTOR('',#17488,1000.);
#5199=VECTOR('',#17489,1000.);
#5200=VECTOR('',#17490,1000.);
#5201=VECTOR('',#17493,1000.);
#5202=VECTOR('',#17494,1000.);
#5203=VECTOR('',#17495,1000.);
#5204=VECTOR('',#17498,1000.);
#5205=VECTOR('',#17499,1000.);
#5206=VECTOR('',#17500,1000.);
#5207=VECTOR('',#17503,1000.);
#5208=VECTOR('',#17504,1000.);
#5209=VECTOR('',#17511,1000.);
#5210=VECTOR('',#17512,1000.);
#5211=VECTOR('',#17513,1000.);
#5212=VECTOR('',#17514,1000.);
#5213=VECTOR('',#17517,1000.);
#5214=VECTOR('',#17518,1000.);
#5215=VECTOR('',#17519,1000.);
#5216=VECTOR('',#17522,1000.);
#5217=VECTOR('',#17523,1000.);
#5218=VECTOR('',#17524,1000.);
#5219=VECTOR('',#17527,1000.);
#5220=VECTOR('',#17528,1000.);
#5221=VECTOR('',#17539,9.00000000000006);
#5222=VECTOR('',#17546,9.00000000000006);
#5223=VECTOR('',#17553,9.00000000000005);
#5224=VECTOR('',#17560,9.00000000000005);
#5225=VECTOR('',#17567,9.00000000000006);
#5226=VECTOR('',#17574,9.00000000000006);
#5227=VECTOR('',#17581,9.00000000000006);
#5228=VECTOR('',#17588,9.00000000000006);
#5229=VECTOR('',#17595,9.00000000000006);
#5230=VECTOR('',#17602,9.00000000000006);
#5231=VECTOR('',#17609,9.00000000000406);
#5232=VECTOR('',#17616,9.00000000000006);
#5233=VECTOR('',#17623,9.00000000000006);
#5234=VECTOR('',#17630,9.00000000000006);
#5235=VECTOR('',#17637,9.00000000000006);
#5236=VECTOR('',#17644,31.0000000000001);
#5237=VECTOR('',#17651,138.);
#5238=VECTOR('',#17658,9.00000000000006);
#5239=VECTOR('',#17663,1000.);
#5240=VECTOR('',#17664,1000.);
#5241=VECTOR('',#17665,1000.);
#5242=VECTOR('',#17666,1000.);
#5243=VECTOR('',#17669,1000.);
#5244=VECTOR('',#17670,1000.);
#5245=VECTOR('',#17671,1000.);
#5246=VECTOR('',#17674,1000.);
#5247=VECTOR('',#17675,1000.);
#5248=VECTOR('',#17676,1000.);
#5249=VECTOR('',#17679,1000.);
#5250=VECTOR('',#17680,1000.);
#5251=VECTOR('',#17689,136.525);
#5252=VECTOR('',#17696,121.435);
#5253=VECTOR('',#17707,30.165);
#5254=VECTOR('',#17714,26.255);
#5255=VECTOR('',#17725,12.4999999999953);
#5256=VECTOR('',#17732,12.4999999999835);
#5257=VECTOR('',#17739,12.4999999999698);
#5258=VECTOR('',#17746,12.4999999999583);
#5259=VECTOR('',#17753,12.4999999999518);
#5260=VECTOR('',#17760,12.4999999999521);
#5261=VECTOR('',#17767,12.499999999959);
#5262=VECTOR('',#17774,12.4999999999705);
#5263=VECTOR('',#17781,12.4999999999835);
#5264=VECTOR('',#17788,12.4999999999946);
#5265=VECTOR('',#17795,12.5000000000006);
#5266=VECTOR('',#17802,12.5);
#5267=VECTOR('',#17809,138.);
#5268=VECTOR('',#17816,203.);
#5269=VECTOR('',#17827,9.50000000000001);
#5270=VECTOR('',#17834,9.50000000000006);
#5271=VECTOR('',#17841,9.50000000000001);
#5272=VECTOR('',#17848,9.50000000000001);
#5273=VECTOR('',#17855,31.);
#5274=VECTOR('',#17862,76.0000000000001);
#5275=VECTOR('',#17875,1000.);
#5276=VECTOR('',#17876,1000.);
#5277=VECTOR('',#17877,1000.);
#5278=VECTOR('',#17878,1000.);
#5279=VECTOR('',#17881,1000.);
#5280=VECTOR('',#17884,1000.);
#5281=VECTOR('',#17889,1000.);
#5282=VECTOR('',#17890,1000.);
#5283=VECTOR('',#17893,1000.);
#5284=VECTOR('',#17896,1000.);
#5285=VECTOR('',#17899,1000.);
#5286=VECTOR('',#17900,1000.);
#5287=VECTOR('',#17903,1000.);
#5288=VECTOR('',#17904,1000.);
#5289=VECTOR('',#17907,1000.);
#5290=VECTOR('',#17910,1000.);
#5291=VECTOR('',#17913,1000.);
#5292=VECTOR('',#17916,1000.);
#5293=VECTOR('',#17919,1000.);
#5294=VECTOR('',#17922,1000.);
#5295=VECTOR('',#17925,1000.);
#5296=VECTOR('',#17930,1000.);
#5297=VECTOR('',#17933,1000.);
#5298=VECTOR('',#17936,1000.);
#5299=VECTOR('',#17939,1000.);
#5300=VECTOR('',#17940,1000.);
#5301=VECTOR('',#17941,1000.);
#5302=VECTOR('',#17944,1000.);
#5303=VECTOR('',#17945,1000.);
#5304=VECTOR('',#17946,1000.);
#5305=VECTOR('',#17949,1000.);
#5306=VECTOR('',#17952,1000.);
#5307=VECTOR('',#17955,1000.);
#5308=VECTOR('',#17958,1000.);
#5309=VECTOR('',#17959,1000.);
#5310=VECTOR('',#17962,1000.);
#5311=VECTOR('',#17965,1000.);
#5312=VECTOR('',#17968,1000.);
#5313=VECTOR('',#17971,1000.);
#5314=VECTOR('',#17974,1000.);
#5315=VECTOR('',#17977,1000.);
#5316=VECTOR('',#17980,1000.);
#5317=VECTOR('',#17985,1000.);
#5318=VECTOR('',#17988,1000.);
#5319=VECTOR('',#17991,1000.);
#5320=VECTOR('',#17994,1000.);
#5321=VECTOR('',#17995,1000.);
#5322=VECTOR('',#17996,1000.);
#5323=VECTOR('',#17999,1000.);
#5324=VECTOR('',#18000,1000.);
#5325=VECTOR('',#18001,1000.);
#5326=VECTOR('',#18004,1000.);
#5327=VECTOR('',#18007,1000.);
#5328=VECTOR('',#18010,1000.);
#5329=VECTOR('',#18013,1000.);
#5330=VECTOR('',#18014,1000.);
#5331=VECTOR('',#18017,1000.);
#5332=VECTOR('',#18020,1000.);
#5333=VECTOR('',#18023,1000.);
#5334=VECTOR('',#18026,1000.);
#5335=VECTOR('',#18029,1000.);
#5336=VECTOR('',#18032,1000.);
#5337=VECTOR('',#18035,1000.);
#5338=VECTOR('',#18042,9.00000000000001);
#5339=VECTOR('',#18049,1000.);
#5340=VECTOR('',#18052,1000.);
#5341=VECTOR('',#18057,1000.);
#5342=VECTOR('',#18062,1000.);
#5343=VECTOR('',#18063,1000.);
#5344=VECTOR('',#18064,1000.);
#5345=VECTOR('',#18067,1000.);
#5346=VECTOR('',#18068,1000.);
#5347=VECTOR('',#18069,1000.);
#5348=VECTOR('',#18072,1000.);
#5349=VECTOR('',#18073,1000.);
#5350=VECTOR('',#18074,1000.);
#5351=VECTOR('',#18077,1000.);
#5352=VECTOR('',#18078,1000.);
#5353=VECTOR('',#18087,9.00000000000001);
#5354=VECTOR('',#18092,1000.);
#5355=VECTOR('',#18093,1000.);
#5356=VECTOR('',#18094,1000.);
#5357=VECTOR('',#18097,1000.);
#5358=VECTOR('',#18098,1000.);
#5359=VECTOR('',#18101,1000.);
#5360=VECTOR('',#18102,1000.);
#5361=VECTOR('',#18103,1000.);
#5362=VECTOR('',#18106,1000.);
#5363=VECTOR('',#18107,1000.);
#5364=VECTOR('',#18110,1000.);
#5365=VECTOR('',#18111,1000.);
#5366=VECTOR('',#18114,1000.);
#5367=VECTOR('',#18117,1000.);
#5368=VECTOR('',#18120,1000.);
#5369=VECTOR('',#18123,1000.);
#5370=VECTOR('',#18130,9.00000000000001);
#5371=VECTOR('',#18137,1000.);
#5372=VECTOR('',#18140,1000.);
#5373=VECTOR('',#18147,1000.);
#5374=VECTOR('',#18150,1000.);
#5375=VECTOR('',#18151,1000.);
#5376=VECTOR('',#18152,1000.);
#5377=VECTOR('',#18155,1000.);
#5378=VECTOR('',#18156,1000.);
#5379=VECTOR('',#18157,1000.);
#5380=VECTOR('',#18160,1000.);
#5381=VECTOR('',#18161,1000.);
#5382=VECTOR('',#18162,1000.);
#5383=VECTOR('',#18165,1000.);
#5384=VECTOR('',#18166,1000.);
#5385=VECTOR('',#18175,9.00000000000001);
#5386=VECTOR('',#18180,1000.);
#5387=VECTOR('',#18181,1000.);
#5388=VECTOR('',#18182,1000.);
#5389=VECTOR('',#18185,1000.);
#5390=VECTOR('',#18186,1000.);
#5391=VECTOR('',#18189,1000.);
#5392=VECTOR('',#18190,1000.);
#5393=VECTOR('',#18191,1000.);
#5394=VECTOR('',#18194,1000.);
#5395=VECTOR('',#18195,1000.);
#5396=VECTOR('',#18198,1000.);
#5397=VECTOR('',#18199,1000.);
#5398=VECTOR('',#18202,1000.);
#5399=VECTOR('',#18205,1000.);
#5400=VECTOR('',#18208,1000.);
#5401=VECTOR('',#18211,1000.);
#5402=VECTOR('',#18218,1000.);
#5403=VECTOR('',#18221,1000.);
#5404=VECTOR('',#18226,1000.);
#5405=VECTOR('',#18229,1000.);
#5406=VECTOR('',#18234,1000.);
#5407=VECTOR('',#18237,1000.);
#5408=VECTOR('',#18242,1000.);
#5409=VECTOR('',#18245,1000.);
#5410=VECTOR('',#18248,1000.);
#5411=VECTOR('',#18249,1000.);
#5412=VECTOR('',#18250,1000.);
#5413=VECTOR('',#18253,1000.);
#5414=VECTOR('',#18254,1000.);
#5415=VECTOR('',#18255,1000.);
#5416=VECTOR('',#18258,1000.);
#5417=VECTOR('',#18261,1000.);
#5418=VECTOR('',#18264,1000.);
#5419=VECTOR('',#18267,1000.);
#5420=VECTOR('',#18268,1000.);
#5421=VECTOR('',#18269,1000.);
#5422=VECTOR('',#18272,1000.);
#5423=VECTOR('',#18273,1000.);
#5424=VECTOR('',#18274,1000.);
#5425=VECTOR('',#18277,1000.);
#5426=VECTOR('',#18280,1000.);
#5427=VECTOR('',#18283,1000.);
#5428=VECTOR('',#18284,1000.);
#5429=VECTOR('',#18285,1000.);
#5430=VECTOR('',#18286,1000.);
#5431=VECTOR('',#18287,1000.);
#5432=VECTOR('',#18288,1000.);
#5433=VECTOR('',#18291,1000.);
#5434=VECTOR('',#18294,1000.);
#5435=VECTOR('',#18297,1000.);
#5436=VECTOR('',#18300,1000.);
#5437=VECTOR('',#18303,1000.);
#5438=VECTOR('',#18306,1000.);
#5439=VECTOR('',#18307,1000.);
#5440=VECTOR('',#18308,1000.);
#5441=VECTOR('',#18309,1000.);
#5442=VECTOR('',#18310,1000.);
#5443=VECTOR('',#18315,1000.);
#5444=VECTOR('',#18318,1000.);
#5445=VECTOR('',#18331,9.00000000000001);
#5446=VECTOR('',#18336,1000.);
#5447=VECTOR('',#18337,1000.);
#5448=VECTOR('',#18338,1000.);
#5449=VECTOR('',#18341,1000.);
#5450=VECTOR('',#18342,1000.);
#5451=VECTOR('',#18345,1000.);
#5452=VECTOR('',#18346,1000.);
#5453=VECTOR('',#18347,1000.);
#5454=VECTOR('',#18350,1000.);
#5455=VECTOR('',#18351,1000.);
#5456=VECTOR('',#18354,1000.);
#5457=VECTOR('',#18355,1000.);
#5458=VECTOR('',#18358,1000.);
#5459=VECTOR('',#18361,1000.);
#5460=VECTOR('',#18364,1000.);
#5461=VECTOR('',#18367,1000.);
#5462=VECTOR('',#18374,9.00000000000001);
#5463=VECTOR('',#18379,1000.);
#5464=VECTOR('',#18380,1000.);
#5465=VECTOR('',#18381,1000.);
#5466=VECTOR('',#18384,1000.);
#5467=VECTOR('',#18385,1000.);
#5468=VECTOR('',#18388,1000.);
#5469=VECTOR('',#18389,1000.);
#5470=VECTOR('',#18390,1000.);
#5471=VECTOR('',#18393,1000.);
#5472=VECTOR('',#18394,1000.);
#5473=VECTOR('',#18397,1000.);
#5474=VECTOR('',#18398,1000.);
#5475=VECTOR('',#18401,1000.);
#5476=VECTOR('',#18404,1000.);
#5477=VECTOR('',#18407,1000.);
#5478=VECTOR('',#18410,1000.);
#5479=VECTOR('',#18417,1000.);
#5480=VECTOR('',#18418,1000.);
#5481=VECTOR('',#18419,1000.);
#5482=VECTOR('',#18420,1000.);
#5483=VECTOR('',#18423,1000.);
#5484=VECTOR('',#18424,1000.);
#5485=VECTOR('',#18425,1000.);
#5486=VECTOR('',#18430,1000.);
#5487=VECTOR('',#18435,1000.);
#5488=VECTOR('',#18436,1000.);
#5489=VECTOR('',#18437,1000.);
#5490=VECTOR('',#18440,1000.);
#5491=VECTOR('',#18441,1000.);
#5492=VECTOR('',#18442,1000.);
#5493=VECTOR('',#18445,1000.);
#5494=VECTOR('',#18446,1000.);
#5495=VECTOR('',#18447,1000.);
#5496=VECTOR('',#18452,1000.);
#5497=VECTOR('',#18457,1000.);
#5498=VECTOR('',#18458,1000.);
#5499=VECTOR('',#18459,1000.);
#5500=VECTOR('',#18462,1000.);
#5501=VECTOR('',#18463,1000.);
#5502=VECTOR('',#18464,1000.);
#5503=VECTOR('',#18467,1000.);
#5504=VECTOR('',#18468,1000.);
#5505=VECTOR('',#18469,1000.);
#5506=VECTOR('',#18472,1000.);
#5507=VECTOR('',#18473,1000.);
#5508=VECTOR('',#18474,1000.);
#5509=VECTOR('',#18477,1000.);
#5510=VECTOR('',#18478,1000.);
#5511=VECTOR('',#18487,9.00000000000001);
#5512=VECTOR('',#18494,1000.);
#5513=VECTOR('',#18497,1000.);
#5514=VECTOR('',#18502,1000.);
#5515=VECTOR('',#18507,1000.);
#5516=VECTOR('',#18508,1000.);
#5517=VECTOR('',#18509,1000.);
#5518=VECTOR('',#18510,1000.);
#5519=VECTOR('',#18513,1000.);
#5520=VECTOR('',#18514,1000.);
#5521=VECTOR('',#18515,1000.);
#5522=VECTOR('',#18516,1000.);
#5523=VECTOR('',#18519,1000.);
#5524=VECTOR('',#18522,1000.);
#5525=VECTOR('',#18525,1000.);
#5526=VECTOR('',#18532,9.00000000000001);
#5527=VECTOR('',#18539,1000.);
#5528=VECTOR('',#18542,1000.);
#5529=VECTOR('',#18549,1000.);
#5530=VECTOR('',#18552,1000.);
#5531=VECTOR('',#18553,1000.);
#5532=VECTOR('',#18554,1000.);
#5533=VECTOR('',#18555,1000.);
#5534=VECTOR('',#18558,1000.);
#5535=VECTOR('',#18559,1000.);
#5536=VECTOR('',#18560,1000.);
#5537=VECTOR('',#18561,1000.);
#5538=VECTOR('',#18564,1000.);
#5539=VECTOR('',#18567,1000.);
#5540=VECTOR('',#18570,1000.);
#5541=VECTOR('',#18595,7.93749999999998);
#5542=VECTOR('',#18600,7.93749999999999);
#5543=VECTOR('',#18605,7.93749999999998);
#5544=VECTOR('',#18616,7.09803);
#5545=VECTOR('',#18623,7.9375);
#5546=VECTOR('',#18626,1000.);
#5547=VECTOR('',#18627,1000.);
#5548=VECTOR('',#18628,1000.);
#5549=VECTOR('',#18631,1000.);
#5550=VECTOR('',#18632,1000.);
#5551=VECTOR('',#18635,1000.);
#5552=VECTOR('',#18636,1000.);
#5553=VECTOR('',#18639,1000.);
#5554=VECTOR('',#18640,1000.);
#5555=VECTOR('',#18643,1000.);
#5556=VECTOR('',#18644,1000.);
#5557=VECTOR('',#18647,1000.);
#5558=VECTOR('',#18684,7.09803);
#5559=VECTOR('',#18691,7.9375);
#5560=VECTOR('',#18694,1000.);
#5561=VECTOR('',#18695,1000.);
#5562=VECTOR('',#18696,1000.);
#5563=VECTOR('',#18699,1000.);
#5564=VECTOR('',#18700,1000.);
#5565=VECTOR('',#18703,1000.);
#5566=VECTOR('',#18704,1000.);
#5567=VECTOR('',#18707,1000.);
#5568=VECTOR('',#18708,1000.);
#5569=VECTOR('',#18711,1000.);
#5570=VECTOR('',#18712,1000.);
#5571=VECTOR('',#18715,1000.);
#5572=VECTOR('',#18752,7.9375);
#5573=VECTOR('',#18761,7.9375);
#5574=VECTOR('',#18768,7.282307);
#5575=VECTOR('',#18773,7.34187);
#5576=VECTOR('',#18776,1000.);
#5577=VECTOR('',#18777,1000.);
#5578=VECTOR('',#18780,1000.);
#5579=VECTOR('',#18783,1000.);
#5580=VECTOR('',#18786,1000.);
#5581=VECTOR('',#18789,1000.);
#5582=VECTOR('',#18848,6.56268467496113);
#5583=VECTOR('',#18853,6.56268467496113);
#5584=VECTOR('',#18856,6.56268467496113);
#5585=VECTOR('',#18859,6.56268467496113);
#5586=VECTOR('',#18862,6.56268467496113);
#5587=VECTOR('',#18865,6.56268467496113);
#5588=VECTOR('',#18868,6.56268467496113);
#5589=VECTOR('',#18871,6.56268467496113);
#5590=VECTOR('',#18874,6.56268467496113);
#5591=VECTOR('',#18877,6.56268467496113);
#5592=VECTOR('',#18880,6.56268467496113);
#5593=VECTOR('',#18883,6.56268467496113);
#5594=VECTOR('',#18886,6.56268467496113);
#5595=VECTOR('',#18889,6.56268467496113);
#5596=VECTOR('',#18892,6.56268467496113);
#5597=VECTOR('',#18895,6.56268467496113);
#5598=VECTOR('',#18898,6.56268467496113);
#5599=VECTOR('',#18901,6.56268467496113);
#5600=VECTOR('',#18904,6.56268467496113);
#5601=VECTOR('',#18907,6.56268467496113);
#5602=VECTOR('',#18910,6.56268467496113);
#5603=VECTOR('',#18913,6.56268467496113);
#5604=VECTOR('',#18916,7.9375);
#5605=VECTOR('',#18917,7.9375);
#5606=VECTOR('',#18918,1000.);
#5607=VECTOR('',#18921,7.9375);
#5608=VECTOR('',#18924,7.9375);
#5609=VECTOR('',#18927,7.9375);
#5610=VECTOR('',#18930,7.9375);
#5611=VECTOR('',#18933,7.9375);
#5612=VECTOR('',#18936,7.9375);
#5613=VECTOR('',#18939,7.9375);
#5614=VECTOR('',#18942,7.9375);
#5615=VECTOR('',#18945,7.9375);
#5616=VECTOR('',#18948,7.9375);
#5617=VECTOR('',#18951,7.9375);
#5618=VECTOR('',#18954,7.9375);
#5619=VECTOR('',#18957,7.9375);
#5620=VECTOR('',#18960,7.9375);
#5621=VECTOR('',#18963,7.9375);
#5622=VECTOR('',#18966,7.9375);
#5623=VECTOR('',#18969,7.9375);
#5624=VECTOR('',#18972,7.9375);
#5625=VECTOR('',#18975,7.9375);
#5626=VECTOR('',#18978,7.9375);
#5627=VECTOR('',#19005,9.);
#5628=VECTOR('',#19014,4.93749999999999);
#5629=VECTOR('',#19027,10.);
#5630=VECTOR('',#19028,10.);
#5631=VECTOR('',#19029,10.);
#5632=VECTOR('',#19052,6.56268467749995);
#5633=VECTOR('',#19057,6.56268467749995);
#5634=VECTOR('',#19060,6.56268467749995);
#5635=VECTOR('',#19063,6.56268467749995);
#5636=VECTOR('',#19066,6.56268467749995);
#5637=VECTOR('',#19071,7.9375);
#5638=VECTOR('',#19076,7.9375);
#5639=VECTOR('',#19081,7.9375);
#5640=VECTOR('',#19084,7.9375);
#5641=VECTOR('',#19087,7.9375);
#5642=VECTOR('',#19090,7.9375);
#5643=VECTOR('',#19097,4.93749999999997);
#5644=VECTOR('',#19104,7.9375);
#5645=VECTOR('',#19109,7.9375);
#5646=VECTOR('',#19128,1000.);
#5647=VECTOR('',#19129,1000.);
#5648=VECTOR('',#19130,1000.);
#5649=VECTOR('',#19131,1000.);
#5650=VECTOR('',#19136,1000.);
#5651=VECTOR('',#19137,1000.);
#5652=VECTOR('',#19138,1000.);
#5653=VECTOR('',#19145,1000.);
#5654=VECTOR('',#19148,1000.);
#5655=VECTOR('',#19151,1000.);
#5656=VECTOR('',#19154,1000.);
#5657=VECTOR('',#19161,1000.);
#5658=VECTOR('',#19164,1000.);
#5659=VECTOR('',#19167,1000.);
#5660=VECTOR('',#19170,1000.);
#5661=VECTOR('',#19177,1000.);
#5662=VECTOR('',#19180,1000.);
#5663=VECTOR('',#19183,1000.);
#5664=VECTOR('',#19222,16.6624);
#5665=VECTOR('',#19229,8.3312);
#5666=VECTOR('',#19280,1000.);
#5667=VECTOR('',#19281,1000.);
#5668=VECTOR('',#19282,1000.);
#5669=VECTOR('',#19283,1000.);
#5670=VECTOR('',#19286,1000.);
#5671=VECTOR('',#19287,1000.);
#5672=VECTOR('',#19288,1000.);
#5673=VECTOR('',#19291,1000.);
#5674=VECTOR('',#19292,1000.);
#5675=VECTOR('',#19293,1000.);
#5676=VECTOR('',#19296,1000.);
#5677=VECTOR('',#19297,1000.);
#5678=VECTOR('',#19306,40.);
#5679=VECTOR('',#19311,1000.);
#5680=VECTOR('',#19312,1000.);
#5681=VECTOR('',#19313,1000.);
#5682=VECTOR('',#19314,1000.);
#5683=VECTOR('',#19317,1000.);
#5684=VECTOR('',#19320,1000.);
#5685=VECTOR('',#19321,1000.);
#5686=VECTOR('',#19324,1000.);
#5687=VECTOR('',#19325,1000.);
#5688=VECTOR('',#19326,1000.);
#5689=VECTOR('',#19329,1000.);
#5690=VECTOR('',#19330,1000.);
#5691=VECTOR('',#19333,1000.);
#5692=VECTOR('',#19336,1000.);
#5693=VECTOR('',#19339,1000.);
#5694=VECTOR('',#19342,1000.);
#5695=VECTOR('',#19349,40.);
#5696=VECTOR('',#19354,1000.);
#5697=VECTOR('',#19355,1000.);
#5698=VECTOR('',#19358,1000.);
#5699=VECTOR('',#19359,1000.);
#5700=VECTOR('',#19360,1000.);
#5701=VECTOR('',#19363,1000.);
#5702=VECTOR('',#19364,1000.);
#5703=VECTOR('',#19365,1000.);
#5704=VECTOR('',#19366,1000.);
#5705=VECTOR('',#19369,1000.);
#5706=VECTOR('',#19372,1000.);
#5707=VECTOR('',#19373,1000.);
#5708=VECTOR('',#19376,1000.);
#5709=VECTOR('',#19379,1000.);
#5710=VECTOR('',#19382,1000.);
#5711=VECTOR('',#19385,1000.);
#5712=VECTOR('',#19392,8.99999999999999);
#5713=VECTOR('',#19399,8.99999999999999);
#5714=VECTOR('',#19406,8.99999999999998);
#5715=VECTOR('',#19413,9.);
#5716=VECTOR('',#19420,8.99999999999999);
#5717=VECTOR('',#19425,1000.);
#5718=VECTOR('',#19426,1000.);
#5719=VECTOR('',#19427,1000.);
#5720=VECTOR('',#19428,1000.);
#5721=VECTOR('',#19429,1000.);
#5722=VECTOR('',#19430,1000.);
#5723=VECTOR('',#19431,1000.);
#5724=VECTOR('',#19432,1000.);
#5725=VECTOR('',#19435,1000.);
#5726=VECTOR('',#19436,1000.);
#5727=VECTOR('',#19437,1000.);
#5728=VECTOR('',#19438,1000.);
#5729=VECTOR('',#19439,1000.);
#5730=VECTOR('',#19440,1000.);
#5731=VECTOR('',#19441,1000.);
#5732=VECTOR('',#19442,1000.);
#5733=VECTOR('',#19445,1000.);
#5734=VECTOR('',#19446,1000.);
#5735=VECTOR('',#19449,1000.);
#5736=VECTOR('',#19452,1000.);
#5737=VECTOR('',#19455,1000.);
#5738=VECTOR('',#19458,1000.);
#5739=VECTOR('',#19461,1000.);
#5740=VECTOR('',#19464,1000.);
#5741=VECTOR('',#19469,1000.);
#5742=VECTOR('',#19470,1000.);
#5743=VECTOR('',#19471,1000.);
#5744=VECTOR('',#19472,1000.);
#5745=VECTOR('',#19475,1000.);
#5746=VECTOR('',#19476,1000.);
#5747=VECTOR('',#19477,1000.);
#5748=VECTOR('',#19480,1000.);
#5749=VECTOR('',#19481,1000.);
#5750=VECTOR('',#19482,1000.);
#5751=VECTOR('',#19485,1000.);
#5752=VECTOR('',#19486,1000.);
#5753=VECTOR('',#19493,1000.);
#5754=VECTOR('',#19494,1000.);
#5755=VECTOR('',#19495,1000.);
#5756=VECTOR('',#19496,1000.);
#5757=VECTOR('',#19499,1000.);
#5758=VECTOR('',#19500,1000.);
#5759=VECTOR('',#19501,1000.);
#5760=VECTOR('',#19504,1000.);
#5761=VECTOR('',#19505,1000.);
#5762=VECTOR('',#19506,1000.);
#5763=VECTOR('',#19509,1000.);
#5764=VECTOR('',#19510,1000.);
#5765=VECTOR('',#19517,1000.);
#5766=VECTOR('',#19518,1000.);
#5767=VECTOR('',#19519,1000.);
#5768=VECTOR('',#19520,1000.);
#5769=VECTOR('',#19523,1000.);
#5770=VECTOR('',#19524,1000.);
#5771=VECTOR('',#19525,1000.);
#5772=VECTOR('',#19528,1000.);
#5773=VECTOR('',#19529,1000.);
#5774=VECTOR('',#19530,1000.);
#5775=VECTOR('',#19533,1000.);
#5776=VECTOR('',#19534,1000.);
#5777=VECTOR('',#19535,1000.);
#5778=VECTOR('',#19538,1000.);
#5779=VECTOR('',#19539,1000.);
#5780=VECTOR('',#19540,1000.);
#5781=VECTOR('',#19543,1000.);
#5782=VECTOR('',#19544,1000.);
#5783=VECTOR('',#19553,8.99999999999997);
#5784=VECTOR('',#19560,8.99999999999999);
#5785=VECTOR('',#19567,8.99999999999997);
#5786=VECTOR('',#19572,1000.);
#5787=VECTOR('',#19573,1000.);
#5788=VECTOR('',#19574,1000.);
#5789=VECTOR('',#19575,1000.);
#5790=VECTOR('',#19578,1000.);
#5791=VECTOR('',#19579,1000.);
#5792=VECTOR('',#19580,1000.);
#5793=VECTOR('',#19581,1000.);
#5794=VECTOR('',#19584,1000.);
#5795=VECTOR('',#19585,1000.);
#5796=VECTOR('',#19588,1000.);
#5797=VECTOR('',#19591,1000.);
#5798=VECTOR('',#19598,8.99999999999998);
#5799=VECTOR('',#19605,9.);
#5800=VECTOR('',#19612,8.99999999999995);
#5801=VECTOR('',#19617,1000.);
#5802=VECTOR('',#19618,1000.);
#5803=VECTOR('',#19619,1000.);
#5804=VECTOR('',#19620,1000.);
#5805=VECTOR('',#19623,1000.);
#5806=VECTOR('',#19624,1000.);
#5807=VECTOR('',#19625,1000.);
#5808=VECTOR('',#19626,1000.);
#5809=VECTOR('',#19629,1000.);
#5810=VECTOR('',#19630,1000.);
#5811=VECTOR('',#19633,1000.);
#5812=VECTOR('',#19636,1000.);
#5813=VECTOR('',#19643,8.99999999999998);
#5814=VECTOR('',#19650,8.99999999999999);
#5815=VECTOR('',#19657,8.99999999999997);
#5816=VECTOR('',#19662,1000.);
#5817=VECTOR('',#19663,1000.);
#5818=VECTOR('',#19664,1000.);
#5819=VECTOR('',#19665,1000.);
#5820=VECTOR('',#19668,1000.);
#5821=VECTOR('',#19669,1000.);
#5822=VECTOR('',#19670,1000.);
#5823=VECTOR('',#19671,1000.);
#5824=VECTOR('',#19674,1000.);
#5825=VECTOR('',#19675,1000.);
#5826=VECTOR('',#19678,1000.);
#5827=VECTOR('',#19681,1000.);
#5828=VECTOR('',#19688,8.99999999999999);
#5829=VECTOR('',#19695,9.);
#5830=VECTOR('',#19702,8.99999999999996);
#5831=VECTOR('',#19707,1000.);
#5832=VECTOR('',#19708,1000.);
#5833=VECTOR('',#19709,1000.);
#5834=VECTOR('',#19710,1000.);
#5835=VECTOR('',#19713,1000.);
#5836=VECTOR('',#19714,1000.);
#5837=VECTOR('',#19715,1000.);
#5838=VECTOR('',#19716,1000.);
#5839=VECTOR('',#19719,1000.);
#5840=VECTOR('',#19720,1000.);
#5841=VECTOR('',#19723,1000.);
#5842=VECTOR('',#19726,1000.);
#5843=VECTOR('',#19731,1000.);
#5844=VECTOR('',#19732,1000.);
#5845=VECTOR('',#19733,1000.);
#5846=VECTOR('',#19734,1000.);
#5847=VECTOR('',#19737,1000.);
#5848=VECTOR('',#19738,1000.);
#5849=VECTOR('',#19739,1000.);
#5850=VECTOR('',#19742,1000.);
#5851=VECTOR('',#19743,1000.);
#5852=VECTOR('',#19744,1000.);
#5853=VECTOR('',#19747,1000.);
#5854=VECTOR('',#19748,1000.);
#5855=VECTOR('',#19755,1000.);
#5856=VECTOR('',#19756,1000.);
#5857=VECTOR('',#19757,1000.);
#5858=VECTOR('',#19758,1000.);
#5859=VECTOR('',#19761,1000.);
#5860=VECTOR('',#19762,1000.);
#5861=VECTOR('',#19763,1000.);
#5862=VECTOR('',#19766,1000.);
#5863=VECTOR('',#19767,1000.);
#5864=VECTOR('',#19768,1000.);
#5865=VECTOR('',#19771,1000.);
#5866=VECTOR('',#19772,1000.);
#5867=VECTOR('',#19779,1000.);
#5868=VECTOR('',#19780,1000.);
#5869=VECTOR('',#19781,1000.);
#5870=VECTOR('',#19782,1000.);
#5871=VECTOR('',#19785,1000.);
#5872=VECTOR('',#19786,1000.);
#5873=VECTOR('',#19787,1000.);
#5874=VECTOR('',#19790,1000.);
#5875=VECTOR('',#19791,1000.);
#5876=VECTOR('',#19792,1000.);
#5877=VECTOR('',#19795,1000.);
#5878=VECTOR('',#19796,1000.);
#5879=VECTOR('',#19803,1000.);
#5880=VECTOR('',#19804,1000.);
#5881=VECTOR('',#19805,1000.);
#5882=VECTOR('',#19806,1000.);
#5883=VECTOR('',#19809,1000.);
#5884=VECTOR('',#19810,1000.);
#5885=VECTOR('',#19811,1000.);
#5886=VECTOR('',#19814,1000.);
#5887=VECTOR('',#19815,1000.);
#5888=VECTOR('',#19816,1000.);
#5889=VECTOR('',#19819,1000.);
#5890=VECTOR('',#19820,1000.);
#5891=VECTOR('',#19827,1000.);
#5892=VECTOR('',#19828,1000.);
#5893=VECTOR('',#19829,1000.);
#5894=VECTOR('',#19830,1000.);
#5895=VECTOR('',#19833,1000.);
#5896=VECTOR('',#19834,1000.);
#5897=VECTOR('',#19835,1000.);
#5898=VECTOR('',#19838,1000.);
#5899=VECTOR('',#19839,1000.);
#5900=VECTOR('',#19840,1000.);
#5901=VECTOR('',#19843,1000.);
#5902=VECTOR('',#19844,1000.);
#5903=VECTOR('',#19853,9.00000000000004);
#5904=VECTOR('',#19860,9.00000000000004);
#5905=VECTOR('',#19867,9.00000000000006);
#5906=VECTOR('',#19874,9.00000000000006);
#5907=VECTOR('',#19879,1000.);
#5908=VECTOR('',#19880,1000.);
#5909=VECTOR('',#19881,1000.);
#5910=VECTOR('',#19882,1000.);
#5911=VECTOR('',#19885,1000.);
#5912=VECTOR('',#19886,1000.);
#5913=VECTOR('',#19887,1000.);
#5914=VECTOR('',#19888,1000.);
#5915=VECTOR('',#19891,1000.);
#5916=VECTOR('',#19892,1000.);
#5917=VECTOR('',#19895,1000.);
#5918=VECTOR('',#19898,1000.);
#5919=VECTOR('',#19905,9.00000000000004);
#5920=VECTOR('',#19912,9.00000000000004);
#5921=VECTOR('',#19919,9.00000000000004);
#5922=VECTOR('',#19926,9.00000000000004);
#5923=VECTOR('',#19933,9.00000000000004);
#5924=VECTOR('',#19940,9.00000000000004);
#5925=VECTOR('',#19945,1000.);
#5926=VECTOR('',#19946,1000.);
#5927=VECTOR('',#19947,1000.);
#5928=VECTOR('',#19948,1000.);
#5929=VECTOR('',#19951,1000.);
#5930=VECTOR('',#19952,1000.);
#5931=VECTOR('',#19953,1000.);
#5932=VECTOR('',#19956,1000.);
#5933=VECTOR('',#19957,1000.);
#5934=VECTOR('',#19958,1000.);
#5935=VECTOR('',#19961,1000.);
#5936=VECTOR('',#19962,1000.);
#5937=VECTOR('',#19969,1000.);
#5938=VECTOR('',#19970,1000.);
#5939=VECTOR('',#19971,1000.);
#5940=VECTOR('',#19972,1000.);
#5941=VECTOR('',#19975,1000.);
#5942=VECTOR('',#19976,1000.);
#5943=VECTOR('',#19977,1000.);
#5944=VECTOR('',#19980,1000.);
#5945=VECTOR('',#19981,1000.);
#5946=VECTOR('',#19982,1000.);
#5947=VECTOR('',#19985,1000.);
#5948=VECTOR('',#19986,1000.);
#5949=VECTOR('',#19987,1000.);
#5950=VECTOR('',#19990,1000.);
#5951=VECTOR('',#19991,1000.);
#5952=VECTOR('',#19992,1000.);
#5953=VECTOR('',#19995,1000.);
#5954=VECTOR('',#19996,1000.);
#5955=VECTOR('',#19997,1000.);
#5956=VECTOR('',#20000,1000.);
#5957=VECTOR('',#20001,1000.);
#5958=VECTOR('',#20008,1000.);
#5959=VECTOR('',#20009,1000.);
#5960=VECTOR('',#20010,1000.);
#5961=VECTOR('',#20011,1000.);
#5962=VECTOR('',#20014,1000.);
#5963=VECTOR('',#20015,1000.);
#5964=VECTOR('',#20016,1000.);
#5965=VECTOR('',#20019,1000.);
#5966=VECTOR('',#20020,1000.);
#5967=VECTOR('',#20021,1000.);
#5968=VECTOR('',#20024,1000.);
#5969=VECTOR('',#20025,1000.);
#5970=VECTOR('',#20026,1000.);
#5971=VECTOR('',#20029,1000.);
#5972=VECTOR('',#20030,1000.);
#5973=VECTOR('',#20031,1000.);
#5974=VECTOR('',#20034,1000.);
#5975=VECTOR('',#20035,1000.);
#5976=VECTOR('',#20036,1000.);
#5977=VECTOR('',#20039,1000.);
#5978=VECTOR('',#20040,1000.);
#5979=VECTOR('',#20047,1000.);
#5980=VECTOR('',#20048,1000.);
#5981=VECTOR('',#20049,1000.);
#5982=VECTOR('',#20050,1000.);
#5983=VECTOR('',#20053,1000.);
#5984=VECTOR('',#20054,1000.);
#5985=VECTOR('',#20055,1000.);
#5986=VECTOR('',#20058,1000.);
#5987=VECTOR('',#20059,1000.);
#5988=VECTOR('',#20060,1000.);
#5989=VECTOR('',#20063,1000.);
#5990=VECTOR('',#20064,1000.);
#5991=VECTOR('',#20065,1000.);
#5992=VECTOR('',#20068,1000.);
#5993=VECTOR('',#20069,1000.);
#5994=VECTOR('',#20070,1000.);
#5995=VECTOR('',#20073,1000.);
#5996=VECTOR('',#20074,1000.);
#5997=VECTOR('',#20075,1000.);
#5998=VECTOR('',#20078,1000.);
#5999=VECTOR('',#20079,1000.);
#6000=VECTOR('',#20086,1000.);
#6001=VECTOR('',#20087,1000.);
#6002=VECTOR('',#20088,1000.);
#6003=VECTOR('',#20089,1000.);
#6004=VECTOR('',#20092,1000.);
#6005=VECTOR('',#20093,1000.);
#6006=VECTOR('',#20094,1000.);
#6007=VECTOR('',#20097,1000.);
#6008=VECTOR('',#20098,1000.);
#6009=VECTOR('',#20099,1000.);
#6010=VECTOR('',#20102,1000.);
#6011=VECTOR('',#20103,1000.);
#6012=VECTOR('',#20104,1000.);
#6013=VECTOR('',#20107,1000.);
#6014=VECTOR('',#20108,1000.);
#6015=VECTOR('',#20109,1000.);
#6016=VECTOR('',#20112,1000.);
#6017=VECTOR('',#20113,1000.);
#6018=VECTOR('',#20114,1000.);
#6019=VECTOR('',#20117,1000.);
#6020=VECTOR('',#20118,1000.);
#6021=VECTOR('',#20125,1000.);
#6022=VECTOR('',#20126,1000.);
#6023=VECTOR('',#20127,1000.);
#6024=VECTOR('',#20128,1000.);
#6025=VECTOR('',#20131,1000.);
#6026=VECTOR('',#20132,1000.);
#6027=VECTOR('',#20133,1000.);
#6028=VECTOR('',#20136,1000.);
#6029=VECTOR('',#20137,1000.);
#6030=VECTOR('',#20138,1000.);
#6031=VECTOR('',#20141,1000.);
#6032=VECTOR('',#20142,1000.);
#6033=VECTOR('',#20143,1000.);
#6034=VECTOR('',#20146,1000.);
#6035=VECTOR('',#20147,1000.);
#6036=VECTOR('',#20148,1000.);
#6037=VECTOR('',#20151,1000.);
#6038=VECTOR('',#20152,1000.);
#6039=VECTOR('',#20153,1000.);
#6040=VECTOR('',#20156,1000.);
#6041=VECTOR('',#20157,1000.);
#6042=VECTOR('',#20164,1000.);
#6043=VECTOR('',#20165,1000.);
#6044=VECTOR('',#20166,1000.);
#6045=VECTOR('',#20167,1000.);
#6046=VECTOR('',#20170,1000.);
#6047=VECTOR('',#20171,1000.);
#6048=VECTOR('',#20172,1000.);
#6049=VECTOR('',#20175,1000.);
#6050=VECTOR('',#20176,1000.);
#6051=VECTOR('',#20177,1000.);
#6052=VECTOR('',#20180,1000.);
#6053=VECTOR('',#20181,1000.);
#6054=VECTOR('',#20182,1000.);
#6055=VECTOR('',#20185,1000.);
#6056=VECTOR('',#20186,1000.);
#6057=VECTOR('',#20187,1000.);
#6058=VECTOR('',#20190,1000.);
#6059=VECTOR('',#20191,1000.);
#6060=VECTOR('',#20192,1000.);
#6061=VECTOR('',#20195,1000.);
#6062=VECTOR('',#20196,1000.);
#6063=VECTOR('',#20203,1000.);
#6064=VECTOR('',#20204,1000.);
#6065=VECTOR('',#20205,1000.);
#6066=VECTOR('',#20206,1000.);
#6067=VECTOR('',#20209,1000.);
#6068=VECTOR('',#20210,1000.);
#6069=VECTOR('',#20211,1000.);
#6070=VECTOR('',#20214,1000.);
#6071=VECTOR('',#20215,1000.);
#6072=VECTOR('',#20216,1000.);
#6073=VECTOR('',#20219,1000.);
#6074=VECTOR('',#20220,1000.);
#6075=VECTOR('',#20221,1000.);
#6076=VECTOR('',#20224,1000.);
#6077=VECTOR('',#20225,1000.);
#6078=VECTOR('',#20226,1000.);
#6079=VECTOR('',#20229,1000.);
#6080=VECTOR('',#20230,1000.);
#6081=VECTOR('',#20231,1000.);
#6082=VECTOR('',#20234,1000.);
#6083=VECTOR('',#20235,1000.);
#6084=VECTOR('',#20242,1000.);
#6085=VECTOR('',#20243,1000.);
#6086=VECTOR('',#20244,1000.);
#6087=VECTOR('',#20245,1000.);
#6088=VECTOR('',#20248,1000.);
#6089=VECTOR('',#20249,1000.);
#6090=VECTOR('',#20250,1000.);
#6091=VECTOR('',#20253,1000.);
#6092=VECTOR('',#20254,1000.);
#6093=VECTOR('',#20255,1000.);
#6094=VECTOR('',#20258,1000.);
#6095=VECTOR('',#20259,1000.);
#6096=VECTOR('',#20260,1000.);
#6097=VECTOR('',#20263,1000.);
#6098=VECTOR('',#20264,1000.);
#6099=VECTOR('',#20265,1000.);
#6100=VECTOR('',#20268,1000.);
#6101=VECTOR('',#20269,1000.);
#6102=VECTOR('',#20270,1000.);
#6103=VECTOR('',#20273,1000.);
#6104=VECTOR('',#20274,1000.);
#6105=VECTOR('',#20281,1000.);
#6106=VECTOR('',#20282,1000.);
#6107=VECTOR('',#20283,1000.);
#6108=VECTOR('',#20284,1000.);
#6109=VECTOR('',#20287,1000.);
#6110=VECTOR('',#20288,1000.);
#6111=VECTOR('',#20289,1000.);
#6112=VECTOR('',#20292,1000.);
#6113=VECTOR('',#20293,1000.);
#6114=VECTOR('',#20294,1000.);
#6115=VECTOR('',#20297,1000.);
#6116=VECTOR('',#20298,1000.);
#6117=VECTOR('',#20299,1000.);
#6118=VECTOR('',#20302,1000.);
#6119=VECTOR('',#20303,1000.);
#6120=VECTOR('',#20304,1000.);
#6121=VECTOR('',#20307,1000.);
#6122=VECTOR('',#20308,1000.);
#6123=VECTOR('',#20309,1000.);
#6124=VECTOR('',#20312,1000.);
#6125=VECTOR('',#20313,1000.);
#6126=VECTOR('',#20320,1000.);
#6127=VECTOR('',#20321,1000.);
#6128=VECTOR('',#20322,1000.);
#6129=VECTOR('',#20323,1000.);
#6130=VECTOR('',#20326,1000.);
#6131=VECTOR('',#20327,1000.);
#6132=VECTOR('',#20328,1000.);
#6133=VECTOR('',#20331,1000.);
#6134=VECTOR('',#20332,1000.);
#6135=VECTOR('',#20333,1000.);
#6136=VECTOR('',#20336,1000.);
#6137=VECTOR('',#20337,1000.);
#6138=VECTOR('',#20338,1000.);
#6139=VECTOR('',#20341,1000.);
#6140=VECTOR('',#20342,1000.);
#6141=VECTOR('',#20343,1000.);
#6142=VECTOR('',#20346,1000.);
#6143=VECTOR('',#20347,1000.);
#6144=VECTOR('',#20348,1000.);
#6145=VECTOR('',#20351,1000.);
#6146=VECTOR('',#20352,1000.);
#6147=VECTOR('',#20359,1000.);
#6148=VECTOR('',#20360,1000.);
#6149=VECTOR('',#20361,1000.);
#6150=VECTOR('',#20362,1000.);
#6151=VECTOR('',#20365,1000.);
#6152=VECTOR('',#20366,1000.);
#6153=VECTOR('',#20367,1000.);
#6154=VECTOR('',#20370,1000.);
#6155=VECTOR('',#20371,1000.);
#6156=VECTOR('',#20372,1000.);
#6157=VECTOR('',#20375,1000.);
#6158=VECTOR('',#20376,1000.);
#6159=VECTOR('',#20377,1000.);
#6160=VECTOR('',#20380,1000.);
#6161=VECTOR('',#20381,1000.);
#6162=VECTOR('',#20382,1000.);
#6163=VECTOR('',#20385,1000.);
#6164=VECTOR('',#20386,1000.);
#6165=VECTOR('',#20387,1000.);
#6166=VECTOR('',#20390,1000.);
#6167=VECTOR('',#20391,1000.);
#6168=VECTOR('',#20400,9.00000000000004);
#6169=VECTOR('',#20407,9.00000000000004);
#6170=VECTOR('',#20414,9.00000000000006);
#6171=VECTOR('',#20421,9.00000000000006);
#6172=VECTOR('',#20426,1000.);
#6173=VECTOR('',#20427,1000.);
#6174=VECTOR('',#20428,1000.);
#6175=VECTOR('',#20429,1000.);
#6176=VECTOR('',#20432,1000.);
#6177=VECTOR('',#20433,1000.);
#6178=VECTOR('',#20434,1000.);
#6179=VECTOR('',#20435,1000.);
#6180=VECTOR('',#20438,1000.);
#6181=VECTOR('',#20439,1000.);
#6182=VECTOR('',#20442,1000.);
#6183=VECTOR('',#20445,1000.);
#6184=VECTOR('',#20450,1000.);
#6185=VECTOR('',#20451,1000.);
#6186=VECTOR('',#20452,1000.);
#6187=VECTOR('',#20453,1000.);
#6188=VECTOR('',#20456,1000.);
#6189=VECTOR('',#20457,1000.);
#6190=VECTOR('',#20458,1000.);
#6191=VECTOR('',#20461,1000.);
#6192=VECTOR('',#20462,1000.);
#6193=VECTOR('',#20463,1000.);
#6194=VECTOR('',#20466,1000.);
#6195=VECTOR('',#20467,1000.);
#6196=VECTOR('',#20474,1000.);
#6197=VECTOR('',#20475,1000.);
#6198=VECTOR('',#20476,1000.);
#6199=VECTOR('',#20477,1000.);
#6200=VECTOR('',#20480,1000.);
#6201=VECTOR('',#20481,1000.);
#6202=VECTOR('',#20482,1000.);
#6203=VECTOR('',#20485,1000.);
#6204=VECTOR('',#20486,1000.);
#6205=VECTOR('',#20487,1000.);
#6206=VECTOR('',#20490,1000.);
#6207=VECTOR('',#20491,1000.);
#6208=VECTOR('',#20498,1000.);
#6209=VECTOR('',#20499,1000.);
#6210=VECTOR('',#20500,1000.);
#6211=VECTOR('',#20501,1000.);
#6212=VECTOR('',#20504,1000.);
#6213=VECTOR('',#20505,1000.);
#6214=VECTOR('',#20506,1000.);
#6215=VECTOR('',#20509,1000.);
#6216=VECTOR('',#20510,1000.);
#6217=VECTOR('',#20511,1000.);
#6218=VECTOR('',#20514,1000.);
#6219=VECTOR('',#20515,1000.);
#6220=VECTOR('',#20522,1000.);
#6221=VECTOR('',#20523,1000.);
#6222=VECTOR('',#20524,1000.);
#6223=VECTOR('',#20525,1000.);
#6224=VECTOR('',#20528,1000.);
#6225=VECTOR('',#20529,1000.);
#6226=VECTOR('',#20530,1000.);
#6227=VECTOR('',#20533,1000.);
#6228=VECTOR('',#20534,1000.);
#6229=VECTOR('',#20535,1000.);
#6230=VECTOR('',#20538,1000.);
#6231=VECTOR('',#20539,1000.);
#6232=VECTOR('',#20546,1000.);
#6233=VECTOR('',#20547,1000.);
#6234=VECTOR('',#20548,1000.);
#6235=VECTOR('',#20549,1000.);
#6236=VECTOR('',#20552,1000.);
#6237=VECTOR('',#20553,1000.);
#6238=VECTOR('',#20554,1000.);
#6239=VECTOR('',#20557,1000.);
#6240=VECTOR('',#20558,1000.);
#6241=VECTOR('',#20559,1000.);
#6242=VECTOR('',#20562,1000.);
#6243=VECTOR('',#20563,1000.);
#6244=VECTOR('',#20570,1000.);
#6245=VECTOR('',#20571,1000.);
#6246=VECTOR('',#20572,1000.);
#6247=VECTOR('',#20573,1000.);
#6248=VECTOR('',#20576,1000.);
#6249=VECTOR('',#20577,1000.);
#6250=VECTOR('',#20578,1000.);
#6251=VECTOR('',#20581,1000.);
#6252=VECTOR('',#20582,1000.);
#6253=VECTOR('',#20583,1000.);
#6254=VECTOR('',#20586,1000.);
#6255=VECTOR('',#20587,1000.);
#6256=VECTOR('',#20594,1000.);
#6257=VECTOR('',#20595,1000.);
#6258=VECTOR('',#20596,1000.);
#6259=VECTOR('',#20597,1000.);
#6260=VECTOR('',#20600,1000.);
#6261=VECTOR('',#20601,1000.);
#6262=VECTOR('',#20602,1000.);
#6263=VECTOR('',#20605,1000.);
#6264=VECTOR('',#20606,1000.);
#6265=VECTOR('',#20607,1000.);
#6266=VECTOR('',#20610,1000.);
#6267=VECTOR('',#20611,1000.);
#6268=VECTOR('',#20618,1000.);
#6269=VECTOR('',#20619,1000.);
#6270=VECTOR('',#20620,1000.);
#6271=VECTOR('',#20621,1000.);
#6272=VECTOR('',#20624,1000.);
#6273=VECTOR('',#20625,1000.);
#6274=VECTOR('',#20626,1000.);
#6275=VECTOR('',#20629,1000.);
#6276=VECTOR('',#20630,1000.);
#6277=VECTOR('',#20631,1000.);
#6278=VECTOR('',#20634,1000.);
#6279=VECTOR('',#20635,1000.);
#6280=VECTOR('',#20642,1000.);
#6281=VECTOR('',#20643,1000.);
#6282=VECTOR('',#20644,1000.);
#6283=VECTOR('',#20645,1000.);
#6284=VECTOR('',#20648,1000.);
#6285=VECTOR('',#20649,1000.);
#6286=VECTOR('',#20650,1000.);
#6287=VECTOR('',#20653,1000.);
#6288=VECTOR('',#20654,1000.);
#6289=VECTOR('',#20655,1000.);
#6290=VECTOR('',#20658,1000.);
#6291=VECTOR('',#20659,1000.);
#6292=VECTOR('',#20666,1000.);
#6293=VECTOR('',#20667,1000.);
#6294=VECTOR('',#20668,1000.);
#6295=VECTOR('',#20669,1000.);
#6296=VECTOR('',#20672,1000.);
#6297=VECTOR('',#20673,1000.);
#6298=VECTOR('',#20674,1000.);
#6299=VECTOR('',#20677,1000.);
#6300=VECTOR('',#20678,1000.);
#6301=VECTOR('',#20679,1000.);
#6302=VECTOR('',#20682,1000.);
#6303=VECTOR('',#20683,1000.);
#6304=VECTOR('',#20690,1000.);
#6305=VECTOR('',#20691,1000.);
#6306=VECTOR('',#20692,1000.);
#6307=VECTOR('',#20693,1000.);
#6308=VECTOR('',#20696,1000.);
#6309=VECTOR('',#20697,1000.);
#6310=VECTOR('',#20698,1000.);
#6311=VECTOR('',#20701,1000.);
#6312=VECTOR('',#20702,1000.);
#6313=VECTOR('',#20703,1000.);
#6314=VECTOR('',#20706,1000.);
#6315=VECTOR('',#20707,1000.);
#6316=VECTOR('',#20714,1000.);
#6317=VECTOR('',#20715,1000.);
#6318=VECTOR('',#20716,1000.);
#6319=VECTOR('',#20717,1000.);
#6320=VECTOR('',#20720,1000.);
#6321=VECTOR('',#20721,1000.);
#6322=VECTOR('',#20722,1000.);
#6323=VECTOR('',#20725,1000.);
#6324=VECTOR('',#20726,1000.);
#6325=VECTOR('',#20727,1000.);
#6326=VECTOR('',#20730,1000.);
#6327=VECTOR('',#20731,1000.);
#6328=VECTOR('',#20738,1000.);
#6329=VECTOR('',#20739,1000.);
#6330=VECTOR('',#20740,1000.);
#6331=VECTOR('',#20741,1000.);
#6332=VECTOR('',#20744,1000.);
#6333=VECTOR('',#20745,1000.);
#6334=VECTOR('',#20746,1000.);
#6335=VECTOR('',#20749,1000.);
#6336=VECTOR('',#20750,1000.);
#6337=VECTOR('',#20751,1000.);
#6338=VECTOR('',#20754,1000.);
#6339=VECTOR('',#20755,1000.);
#6340=VECTOR('',#20762,1000.);
#6341=VECTOR('',#20763,1000.);
#6342=VECTOR('',#20764,1000.);
#6343=VECTOR('',#20765,1000.);
#6344=VECTOR('',#20768,1000.);
#6345=VECTOR('',#20769,1000.);
#6346=VECTOR('',#20770,1000.);
#6347=VECTOR('',#20773,1000.);
#6348=VECTOR('',#20774,1000.);
#6349=VECTOR('',#20775,1000.);
#6350=VECTOR('',#20778,1000.);
#6351=VECTOR('',#20779,1000.);
#6352=VECTOR('',#20786,1000.);
#6353=VECTOR('',#20787,1000.);
#6354=VECTOR('',#20788,1000.);
#6355=VECTOR('',#20789,1000.);
#6356=VECTOR('',#20792,1000.);
#6357=VECTOR('',#20793,1000.);
#6358=VECTOR('',#20794,1000.);
#6359=VECTOR('',#20797,1000.);
#6360=VECTOR('',#20798,1000.);
#6361=VECTOR('',#20799,1000.);
#6362=VECTOR('',#20802,1000.);
#6363=VECTOR('',#20803,1000.);
#6364=VECTOR('',#20810,1000.);
#6365=VECTOR('',#20811,1000.);
#6366=VECTOR('',#20812,1000.);
#6367=VECTOR('',#20813,1000.);
#6368=VECTOR('',#20816,1000.);
#6369=VECTOR('',#20817,1000.);
#6370=VECTOR('',#20818,1000.);
#6371=VECTOR('',#20821,1000.);
#6372=VECTOR('',#20822,1000.);
#6373=VECTOR('',#20823,1000.);
#6374=VECTOR('',#20826,1000.);
#6375=VECTOR('',#20827,1000.);
#6376=VECTOR('',#20834,1000.);
#6377=VECTOR('',#20835,1000.);
#6378=VECTOR('',#20836,1000.);
#6379=VECTOR('',#20837,1000.);
#6380=VECTOR('',#20840,1000.);
#6381=VECTOR('',#20841,1000.);
#6382=VECTOR('',#20842,1000.);
#6383=VECTOR('',#20845,1000.);
#6384=VECTOR('',#20846,1000.);
#6385=VECTOR('',#20847,1000.);
#6386=VECTOR('',#20850,1000.);
#6387=VECTOR('',#20851,1000.);
#6388=VECTOR('',#20858,1000.);
#6389=VECTOR('',#20859,1000.);
#6390=VECTOR('',#20860,1000.);
#6391=VECTOR('',#20861,1000.);
#6392=VECTOR('',#20864,1000.);
#6393=VECTOR('',#20865,1000.);
#6394=VECTOR('',#20866,1000.);
#6395=VECTOR('',#20869,1000.);
#6396=VECTOR('',#20870,1000.);
#6397=VECTOR('',#20871,1000.);
#6398=VECTOR('',#20874,1000.);
#6399=VECTOR('',#20875,1000.);
#6400=VECTOR('',#20882,1000.);
#6401=VECTOR('',#20883,1000.);
#6402=VECTOR('',#20884,1000.);
#6403=VECTOR('',#20885,1000.);
#6404=VECTOR('',#20888,1000.);
#6405=VECTOR('',#20889,1000.);
#6406=VECTOR('',#20890,1000.);
#6407=VECTOR('',#20893,1000.);
#6408=VECTOR('',#20894,1000.);
#6409=VECTOR('',#20895,1000.);
#6410=VECTOR('',#20898,1000.);
#6411=VECTOR('',#20899,1000.);
#6412=VECTOR('',#20906,1000.);
#6413=VECTOR('',#20907,1000.);
#6414=VECTOR('',#20908,1000.);
#6415=VECTOR('',#20909,1000.);
#6416=VECTOR('',#20912,1000.);
#6417=VECTOR('',#20913,1000.);
#6418=VECTOR('',#20914,1000.);
#6419=VECTOR('',#20917,1000.);
#6420=VECTOR('',#20918,1000.);
#6421=VECTOR('',#20919,1000.);
#6422=VECTOR('',#20922,1000.);
#6423=VECTOR('',#20923,1000.);
#6424=VECTOR('',#20930,1000.);
#6425=VECTOR('',#20931,1000.);
#6426=VECTOR('',#20932,1000.);
#6427=VECTOR('',#20933,1000.);
#6428=VECTOR('',#20936,1000.);
#6429=VECTOR('',#20937,1000.);
#6430=VECTOR('',#20938,1000.);
#6431=VECTOR('',#20941,1000.);
#6432=VECTOR('',#20942,1000.);
#6433=VECTOR('',#20943,1000.);
#6434=VECTOR('',#20946,1000.);
#6435=VECTOR('',#20947,1000.);
#6436=VECTOR('',#20954,1000.);
#6437=VECTOR('',#20955,1000.);
#6438=VECTOR('',#20956,1000.);
#6439=VECTOR('',#20957,1000.);
#6440=VECTOR('',#20960,1000.);
#6441=VECTOR('',#20961,1000.);
#6442=VECTOR('',#20962,1000.);
#6443=VECTOR('',#20965,1000.);
#6444=VECTOR('',#20966,1000.);
#6445=VECTOR('',#20967,1000.);
#6446=VECTOR('',#20970,1000.);
#6447=VECTOR('',#20971,1000.);
#6448=VECTOR('',#20996,13.5);
#6449=VECTOR('',#21009,6.8985);
#6450=VECTOR('',#21014,8.);
#6451=VECTOR('',#21021,1000.);
#6452=VECTOR('',#21022,1000.);
#6453=VECTOR('',#21025,1000.);
#6454=VECTOR('',#21026,1000.);
#6455=VECTOR('',#21029,1000.);
#6456=VECTOR('',#21030,1000.);
#6457=VECTOR('',#21033,1000.);
#6458=VECTOR('',#21034,1000.);
#6459=VECTOR('',#21037,1000.);
#6460=VECTOR('',#21038,1000.);
#6461=VECTOR('',#21041,1000.);
#6462=VECTOR('',#21042,1000.);
#6463=VECTOR('',#21071,1000.);
#6464=VECTOR('',#21072,1000.);
#6465=VECTOR('',#21075,1000.);
#6466=VECTOR('',#21078,1000.);
#6467=VECTOR('',#21081,1000.);
#6468=VECTOR('',#21084,1000.);
#6469=VECTOR('',#21093,15.);
#6470=VECTOR('',#21100,8.49999999999999);
#6471=VECTOR('',#21113,8.);
#6472=VECTOR('',#21122,8.);
#6473=VECTOR('',#21129,6.9);
#6474=VECTOR('',#21134,7.);
#6475=VECTOR('',#21137,1000.);
#6476=VECTOR('',#21138,1000.);
#6477=VECTOR('',#21141,1000.);
#6478=VECTOR('',#21144,1000.);
#6479=VECTOR('',#21147,1000.);
#6480=VECTOR('',#21150,1000.);
#6481=VERTEX_POINT('',#21312);
#6482=VERTEX_POINT('',#21313);
#6483=VERTEX_POINT('',#21315);
#6484=VERTEX_POINT('',#21317);
#6485=VERTEX_POINT('',#21321);
#6486=VERTEX_POINT('',#21323);
#6487=VERTEX_POINT('',#21327);
#6488=VERTEX_POINT('',#21329);
#6489=VERTEX_POINT('',#21336);
#6490=VERTEX_POINT('',#21337);
#6491=VERTEX_POINT('',#21339);
#6492=VERTEX_POINT('',#21341);
#6493=VERTEX_POINT('',#21345);
#6494=VERTEX_POINT('',#21346);
#6495=VERTEX_POINT('',#21348);
#6496=VERTEX_POINT('',#21350);
#6497=VERTEX_POINT('',#21362);
#6498=VERTEX_POINT('',#21363);
#6499=VERTEX_POINT('',#21365);
#6500=VERTEX_POINT('',#21367);
#6501=VERTEX_POINT('',#21371);
#6502=VERTEX_POINT('',#21373);
#6503=VERTEX_POINT('',#21377);
#6504=VERTEX_POINT('',#21379);
#6505=VERTEX_POINT('',#21383);
#6506=VERTEX_POINT('',#21385);
#6507=VERTEX_POINT('',#21389);
#6508=VERTEX_POINT('',#21391);
#6509=VERTEX_POINT('',#21400);
#6510=VERTEX_POINT('',#21401);
#6511=VERTEX_POINT('',#21403);
#6512=VERTEX_POINT('',#21405);
#6513=VERTEX_POINT('',#21409);
#6514=VERTEX_POINT('',#21411);
#6515=VERTEX_POINT('',#21415);
#6516=VERTEX_POINT('',#21417);
#6517=VERTEX_POINT('',#21421);
#6518=VERTEX_POINT('',#21423);
#6519=VERTEX_POINT('',#21427);
#6520=VERTEX_POINT('',#21429);
#6521=VERTEX_POINT('',#21438);
#6522=VERTEX_POINT('',#21440);
#6523=VERTEX_POINT('',#21444);
#6524=VERTEX_POINT('',#21446);
#6525=VERTEX_POINT('',#21450);
#6526=VERTEX_POINT('',#21452);
#6527=VERTEX_POINT('',#21456);
#6528=VERTEX_POINT('',#21458);
#6529=VERTEX_POINT('',#21462);
#6530=VERTEX_POINT('',#21464);
#6531=VERTEX_POINT('',#21468);
#6532=VERTEX_POINT('',#21470);
#6533=VERTEX_POINT('',#21474);
#6534=VERTEX_POINT('',#21475);
#6535=VERTEX_POINT('',#21477);
#6536=VERTEX_POINT('',#21479);
#6537=VERTEX_POINT('',#21483);
#6538=VERTEX_POINT('',#21484);
#6539=VERTEX_POINT('',#21486);
#6540=VERTEX_POINT('',#21488);
#6541=VERTEX_POINT('',#21500);
#6542=VERTEX_POINT('',#21502);
#6543=VERTEX_POINT('',#21506);
#6544=VERTEX_POINT('',#21508);
#6545=VERTEX_POINT('',#21512);
#6546=VERTEX_POINT('',#21514);
#6547=VERTEX_POINT('',#21518);
#6548=VERTEX_POINT('',#21520);
#6549=VERTEX_POINT('',#21524);
#6550=VERTEX_POINT('',#21526);
#6551=VERTEX_POINT('',#21530);
#6552=VERTEX_POINT('',#21531);
#6553=VERTEX_POINT('',#21533);
#6554=VERTEX_POINT('',#21535);
#6555=VERTEX_POINT('',#21539);
#6556=VERTEX_POINT('',#21541);
#6557=VERTEX_POINT('',#21545);
#6558=VERTEX_POINT('',#21547);
#6559=VERTEX_POINT('',#21556);
#6560=VERTEX_POINT('',#21558);
#6561=VERTEX_POINT('',#21562);
#6562=VERTEX_POINT('',#21564);
#6563=VERTEX_POINT('',#21568);
#6564=VERTEX_POINT('',#21570);
#6565=VERTEX_POINT('',#21574);
#6566=VERTEX_POINT('',#21576);
#6567=VERTEX_POINT('',#21580);
#6568=VERTEX_POINT('',#21582);
#6569=VERTEX_POINT('',#21586);
#6570=VERTEX_POINT('',#21587);
#6571=VERTEX_POINT('',#21589);
#6572=VERTEX_POINT('',#21591);
#6573=VERTEX_POINT('',#21595);
#6574=VERTEX_POINT('',#21597);
#6575=VERTEX_POINT('',#21601);
#6576=VERTEX_POINT('',#21603);
#6577=VERTEX_POINT('',#21612);
#6578=VERTEX_POINT('',#21613);
#6579=VERTEX_POINT('',#21615);
#6580=VERTEX_POINT('',#21617);
#6581=VERTEX_POINT('',#21621);
#6582=VERTEX_POINT('',#21623);
#6583=VERTEX_POINT('',#21627);
#6584=VERTEX_POINT('',#21629);
#6585=VERTEX_POINT('',#21638);
#6586=VERTEX_POINT('',#21639);
#6587=VERTEX_POINT('',#21641);
#6588=VERTEX_POINT('',#21643);
#6589=VERTEX_POINT('',#21647);
#6590=VERTEX_POINT('',#21649);
#6591=VERTEX_POINT('',#21653);
#6592=VERTEX_POINT('',#21655);
#6593=VERTEX_POINT('',#21664);
#6594=VERTEX_POINT('',#21665);
#6595=VERTEX_POINT('',#21667);
#6596=VERTEX_POINT('',#21669);
#6597=VERTEX_POINT('',#21673);
#6598=VERTEX_POINT('',#21675);
#6599=VERTEX_POINT('',#21679);
#6600=VERTEX_POINT('',#21681);
#6601=VERTEX_POINT('',#21691);
#6602=VERTEX_POINT('',#21693);
#6603=VERTEX_POINT('',#21697);
#6604=VERTEX_POINT('',#21699);
#6605=VERTEX_POINT('',#21703);
#6606=VERTEX_POINT('',#21705);
#6607=VERTEX_POINT('',#21709);
#6608=VERTEX_POINT('',#21711);
#6609=VERTEX_POINT('',#21715);
#6610=VERTEX_POINT('',#21717);
#6611=VERTEX_POINT('',#21721);
#6612=VERTEX_POINT('',#21723);
#6613=VERTEX_POINT('',#21727);
#6614=VERTEX_POINT('',#21729);
#6615=VERTEX_POINT('',#21733);
#6616=VERTEX_POINT('',#21735);
#6617=VERTEX_POINT('',#21739);
#6618=VERTEX_POINT('',#21741);
#6619=VERTEX_POINT('',#21745);
#6620=VERTEX_POINT('',#21747);
#6621=VERTEX_POINT('',#21751);
#6622=VERTEX_POINT('',#21753);
#6623=VERTEX_POINT('',#21757);
#6624=VERTEX_POINT('',#21759);
#6625=VERTEX_POINT('',#21763);
#6626=VERTEX_POINT('',#21765);
#6627=VERTEX_POINT('',#21769);
#6628=VERTEX_POINT('',#21771);
#6629=VERTEX_POINT('',#21775);
#6630=VERTEX_POINT('',#21777);
#6631=VERTEX_POINT('',#21781);
#6632=VERTEX_POINT('',#21783);
#6633=VERTEX_POINT('',#21787);
#6634=VERTEX_POINT('',#21789);
#6635=VERTEX_POINT('',#21793);
#6636=VERTEX_POINT('',#21795);
#6637=VERTEX_POINT('',#21799);
#6638=VERTEX_POINT('',#21800);
#6639=VERTEX_POINT('',#21802);
#6640=VERTEX_POINT('',#21804);
#6641=VERTEX_POINT('',#21808);
#6642=VERTEX_POINT('',#21810);
#6643=VERTEX_POINT('',#21814);
#6644=VERTEX_POINT('',#21816);
#6645=VERTEX_POINT('',#21825);
#6646=VERTEX_POINT('',#21827);
#6647=VERTEX_POINT('',#21831);
#6648=VERTEX_POINT('',#21833);
#6649=VERTEX_POINT('',#21839);
#6650=VERTEX_POINT('',#21841);
#6651=VERTEX_POINT('',#21845);
#6652=VERTEX_POINT('',#21847);
#6653=VERTEX_POINT('',#21853);
#6654=VERTEX_POINT('',#21855);
#6655=VERTEX_POINT('',#21859);
#6656=VERTEX_POINT('',#21861);
#6657=VERTEX_POINT('',#21865);
#6658=VERTEX_POINT('',#21867);
#6659=VERTEX_POINT('',#21871);
#6660=VERTEX_POINT('',#21873);
#6661=VERTEX_POINT('',#21877);
#6662=VERTEX_POINT('',#21879);
#6663=VERTEX_POINT('',#21883);
#6664=VERTEX_POINT('',#21885);
#6665=VERTEX_POINT('',#21889);
#6666=VERTEX_POINT('',#21891);
#6667=VERTEX_POINT('',#21895);
#6668=VERTEX_POINT('',#21897);
#6669=VERTEX_POINT('',#21901);
#6670=VERTEX_POINT('',#21903);
#6671=VERTEX_POINT('',#21907);
#6672=VERTEX_POINT('',#21909);
#6673=VERTEX_POINT('',#21913);
#6674=VERTEX_POINT('',#21915);
#6675=VERTEX_POINT('',#21919);
#6676=VERTEX_POINT('',#21921);
#6677=VERTEX_POINT('',#21925);
#6678=VERTEX_POINT('',#21927);
#6679=VERTEX_POINT('',#21931);
#6680=VERTEX_POINT('',#21933);
#6681=VERTEX_POINT('',#21939);
#6682=VERTEX_POINT('',#21941);
#6683=VERTEX_POINT('',#21945);
#6684=VERTEX_POINT('',#21947);
#6685=VERTEX_POINT('',#21951);
#6686=VERTEX_POINT('',#21953);
#6687=VERTEX_POINT('',#21957);
#6688=VERTEX_POINT('',#21959);
#6689=VERTEX_POINT('',#21963);
#6690=VERTEX_POINT('',#21965);
#6691=VERTEX_POINT('',#21969);
#6692=VERTEX_POINT('',#21971);
#6693=VERTEX_POINT('',#21979);
#6694=VERTEX_POINT('',#21980);
#6695=VERTEX_POINT('',#21982);
#6696=VERTEX_POINT('',#21984);
#6697=VERTEX_POINT('',#21986);
#6698=VERTEX_POINT('',#21988);
#6699=VERTEX_POINT('',#21990);
#6700=VERTEX_POINT('',#21992);
#6701=VERTEX_POINT('',#21994);
#6702=VERTEX_POINT('',#21998);
#6703=VERTEX_POINT('',#21999);
#6704=VERTEX_POINT('',#22001);
#6705=VERTEX_POINT('',#22003);
#6706=VERTEX_POINT('',#22005);
#6707=VERTEX_POINT('',#22007);
#6708=VERTEX_POINT('',#22009);
#6709=VERTEX_POINT('',#22011);
#6710=VERTEX_POINT('',#22013);
#6711=VERTEX_POINT('',#22035);
#6712=VERTEX_POINT('',#22036);
#6713=VERTEX_POINT('',#22038);
#6714=VERTEX_POINT('',#22040);
#6715=VERTEX_POINT('',#22042);
#6716=VERTEX_POINT('',#22044);
#6717=VERTEX_POINT('',#22046);
#6718=VERTEX_POINT('',#22048);
#6719=VERTEX_POINT('',#22050);
#6720=VERTEX_POINT('',#22054);
#6721=VERTEX_POINT('',#22055);
#6722=VERTEX_POINT('',#22057);
#6723=VERTEX_POINT('',#22059);
#6724=VERTEX_POINT('',#22061);
#6725=VERTEX_POINT('',#22063);
#6726=VERTEX_POINT('',#22065);
#6727=VERTEX_POINT('',#22067);
#6728=VERTEX_POINT('',#22069);
#6729=VERTEX_POINT('',#22091);
#6730=VERTEX_POINT('',#22092);
#6731=VERTEX_POINT('',#22094);
#6732=VERTEX_POINT('',#22096);
#6733=VERTEX_POINT('',#22098);
#6734=VERTEX_POINT('',#22100);
#6735=VERTEX_POINT('',#22102);
#6736=VERTEX_POINT('',#22104);
#6737=VERTEX_POINT('',#22106);
#6738=VERTEX_POINT('',#22110);
#6739=VERTEX_POINT('',#22111);
#6740=VERTEX_POINT('',#22113);
#6741=VERTEX_POINT('',#22115);
#6742=VERTEX_POINT('',#22117);
#6743=VERTEX_POINT('',#22119);
#6744=VERTEX_POINT('',#22121);
#6745=VERTEX_POINT('',#22123);
#6746=VERTEX_POINT('',#22125);
#6747=VERTEX_POINT('',#22147);
#6748=VERTEX_POINT('',#22149);
#6749=VERTEX_POINT('',#22153);
#6750=VERTEX_POINT('',#22154);
#6751=VERTEX_POINT('',#22156);
#6752=VERTEX_POINT('',#22158);
#6753=VERTEX_POINT('',#22162);
#6754=VERTEX_POINT('',#22164);
#6755=VERTEX_POINT('',#22168);
#6756=VERTEX_POINT('',#22170);
#6757=VERTEX_POINT('',#22174);
#6758=VERTEX_POINT('',#22176);
#6759=VERTEX_POINT('',#22180);
#6760=VERTEX_POINT('',#22182);
#6761=VERTEX_POINT('',#22191);
#6762=VERTEX_POINT('',#22193);
#6763=VERTEX_POINT('',#22197);
#6764=VERTEX_POINT('',#22198);
#6765=VERTEX_POINT('',#22200);
#6766=VERTEX_POINT('',#22202);
#6767=VERTEX_POINT('',#22204);
#6768=VERTEX_POINT('',#22206);
#6769=VERTEX_POINT('',#22210);
#6770=VERTEX_POINT('',#22211);
#6771=VERTEX_POINT('',#22213);
#6772=VERTEX_POINT('',#22215);
#6773=VERTEX_POINT('',#22217);
#6774=VERTEX_POINT('',#22219);
#6775=VERTEX_POINT('',#22235);
#6776=VERTEX_POINT('',#22237);
#6777=VERTEX_POINT('',#22241);
#6778=VERTEX_POINT('',#22242);
#6779=VERTEX_POINT('',#22244);
#6780=VERTEX_POINT('',#22246);
#6781=VERTEX_POINT('',#22250);
#6782=VERTEX_POINT('',#22252);
#6783=VERTEX_POINT('',#22256);
#6784=VERTEX_POINT('',#22258);
#6785=VERTEX_POINT('',#22262);
#6786=VERTEX_POINT('',#22264);
#6787=VERTEX_POINT('',#22268);
#6788=VERTEX_POINT('',#22270);
#6789=VERTEX_POINT('',#22279);
#6790=VERTEX_POINT('',#22281);
#6791=VERTEX_POINT('',#22285);
#6792=VERTEX_POINT('',#22286);
#6793=VERTEX_POINT('',#22288);
#6794=VERTEX_POINT('',#22290);
#6795=VERTEX_POINT('',#22292);
#6796=VERTEX_POINT('',#22294);
#6797=VERTEX_POINT('',#22298);
#6798=VERTEX_POINT('',#22299);
#6799=VERTEX_POINT('',#22301);
#6800=VERTEX_POINT('',#22303);
#6801=VERTEX_POINT('',#22305);
#6802=VERTEX_POINT('',#22307);
#6803=VERTEX_POINT('',#22323);
#6804=VERTEX_POINT('',#22324);
#6805=VERTEX_POINT('',#22326);
#6806=VERTEX_POINT('',#22328);
#6807=VERTEX_POINT('',#22332);
#6808=VERTEX_POINT('',#22333);
#6809=VERTEX_POINT('',#22335);
#6810=VERTEX_POINT('',#22337);
#6811=VERTEX_POINT('',#22341);
#6812=VERTEX_POINT('',#22342);
#6813=VERTEX_POINT('',#22344);
#6814=VERTEX_POINT('',#22346);
#6815=VERTEX_POINT('',#22350);
#6816=VERTEX_POINT('',#22351);
#6817=VERTEX_POINT('',#22353);
#6818=VERTEX_POINT('',#22355);
#6819=VERTEX_POINT('',#22359);
#6820=VERTEX_POINT('',#22361);
#6821=VERTEX_POINT('',#22365);
#6822=VERTEX_POINT('',#22367);
#6823=VERTEX_POINT('',#22371);
#6824=VERTEX_POINT('',#22372);
#6825=VERTEX_POINT('',#22374);
#6826=VERTEX_POINT('',#22376);
#6827=VERTEX_POINT('',#22378);
#6828=VERTEX_POINT('',#22380);
#6829=VERTEX_POINT('',#22382);
#6830=VERTEX_POINT('',#22384);
#6831=VERTEX_POINT('',#22386);
#6832=VERTEX_POINT('',#22390);
#6833=VERTEX_POINT('',#22392);
#6834=VERTEX_POINT('',#22394);
#6835=VERTEX_POINT('',#22396);
#6836=VERTEX_POINT('',#22398);
#6837=VERTEX_POINT('',#22400);
#6838=VERTEX_POINT('',#22405);
#6839=VERTEX_POINT('',#22425);
#6840=VERTEX_POINT('',#22429);
#6841=VERTEX_POINT('',#22439);
#6842=VERTEX_POINT('',#22441);
#6843=VERTEX_POINT('',#22445);
#6844=VERTEX_POINT('',#22446);
#6845=VERTEX_POINT('',#22448);
#6846=VERTEX_POINT('',#22450);
#6847=VERTEX_POINT('',#22452);
#6848=VERTEX_POINT('',#22454);
#6849=VERTEX_POINT('',#22458);
#6850=VERTEX_POINT('',#22459);
#6851=VERTEX_POINT('',#22461);
#6852=VERTEX_POINT('',#22463);
#6853=VERTEX_POINT('',#22465);
#6854=VERTEX_POINT('',#22467);
#6855=VERTEX_POINT('',#22483);
#6856=VERTEX_POINT('',#22485);
#6857=VERTEX_POINT('',#22489);
#6858=VERTEX_POINT('',#22490);
#6859=VERTEX_POINT('',#22492);
#6860=VERTEX_POINT('',#22494);
#6861=VERTEX_POINT('',#22496);
#6862=VERTEX_POINT('',#22498);
#6863=VERTEX_POINT('',#22502);
#6864=VERTEX_POINT('',#22503);
#6865=VERTEX_POINT('',#22505);
#6866=VERTEX_POINT('',#22507);
#6867=VERTEX_POINT('',#22509);
#6868=VERTEX_POINT('',#22511);
#6869=VERTEX_POINT('',#22528);
#6870=VERTEX_POINT('',#22529);
#6871=VERTEX_POINT('',#22531);
#6872=VERTEX_POINT('',#22533);
#6873=VERTEX_POINT('',#22537);
#6874=VERTEX_POINT('',#22539);
#6875=VERTEX_POINT('',#22543);
#6876=VERTEX_POINT('',#22545);
#6877=VERTEX_POINT('',#22549);
#6878=VERTEX_POINT('',#22551);
#6879=VERTEX_POINT('',#22555);
#6880=VERTEX_POINT('',#22557);
#6881=VERTEX_POINT('',#22561);
#6882=VERTEX_POINT('',#22563);
#6883=VERTEX_POINT('',#22567);
#6884=VERTEX_POINT('',#22569);
#6885=VERTEX_POINT('',#22573);
#6886=VERTEX_POINT('',#22575);
#6887=VERTEX_POINT('',#22579);
#6888=VERTEX_POINT('',#22581);
#6889=VERTEX_POINT('',#22585);
#6890=VERTEX_POINT('',#22587);
#6891=VERTEX_POINT('',#22591);
#6892=VERTEX_POINT('',#22593);
#6893=VERTEX_POINT('',#22602);
#6894=VERTEX_POINT('',#22604);
#6895=VERTEX_POINT('',#22608);
#6896=VERTEX_POINT('',#22609);
#6897=VERTEX_POINT('',#22611);
#6898=VERTEX_POINT('',#22613);
#6899=VERTEX_POINT('',#22617);
#6900=VERTEX_POINT('',#22619);
#6901=VERTEX_POINT('',#22623);
#6902=VERTEX_POINT('',#22625);
#6903=VERTEX_POINT('',#22627);
#6904=VERTEX_POINT('',#22631);
#6905=VERTEX_POINT('',#22633);
#6906=VERTEX_POINT('',#22635);
#6907=VERTEX_POINT('',#22646);
#6908=VERTEX_POINT('',#22648);
#6909=VERTEX_POINT('',#22652);
#6910=VERTEX_POINT('',#22653);
#6911=VERTEX_POINT('',#22655);
#6912=VERTEX_POINT('',#22657);
#6913=VERTEX_POINT('',#22661);
#6914=VERTEX_POINT('',#22663);
#6915=VERTEX_POINT('',#22667);
#6916=VERTEX_POINT('',#22669);
#6917=VERTEX_POINT('',#22671);
#6918=VERTEX_POINT('',#22675);
#6919=VERTEX_POINT('',#22677);
#6920=VERTEX_POINT('',#22679);
#6921=VERTEX_POINT('',#22690);
#6922=VERTEX_POINT('',#22691);
#6923=VERTEX_POINT('',#22693);
#6924=VERTEX_POINT('',#22698);
#6925=VERTEX_POINT('',#22700);
#6926=VERTEX_POINT('',#22702);
#6927=VERTEX_POINT('',#22706);
#6928=VERTEX_POINT('',#22712);
#6929=VERTEX_POINT('',#22719);
#6930=VERTEX_POINT('',#22721);
#6931=VERTEX_POINT('',#22725);
#6932=VERTEX_POINT('',#22729);
#6933=VERTEX_POINT('',#22730);
#6934=VERTEX_POINT('',#22734);
#6935=VERTEX_POINT('',#22736);
#6936=VERTEX_POINT('',#22738);
#6937=VERTEX_POINT('',#22744);
#6938=VERTEX_POINT('',#22745);
#6939=VERTEX_POINT('',#22749);
#6940=VERTEX_POINT('',#22756);
#6941=VERTEX_POINT('',#22757);
#6942=VERTEX_POINT('',#22761);
#6943=VERTEX_POINT('',#22768);
#6944=VERTEX_POINT('',#22769);
#6945=VERTEX_POINT('',#22773);
#6946=VERTEX_POINT('',#22780);
#6947=VERTEX_POINT('',#22781);
#6948=VERTEX_POINT('',#22785);
#6949=VERTEX_POINT('',#22792);
#6950=VERTEX_POINT('',#22817);
#6951=VERTEX_POINT('',#22819);
#6952=VERTEX_POINT('',#22823);
#6953=VERTEX_POINT('',#22827);
#6954=VERTEX_POINT('',#22828);
#6955=VERTEX_POINT('',#22832);
#6956=VERTEX_POINT('',#22834);
#6957=VERTEX_POINT('',#22836);
#6958=VERTEX_POINT('',#22842);
#6959=VERTEX_POINT('',#22843);
#6960=VERTEX_POINT('',#22847);
#6961=VERTEX_POINT('',#22854);
#6962=VERTEX_POINT('',#22855);
#6963=VERTEX_POINT('',#22859);
#6964=VERTEX_POINT('',#22866);
#6965=VERTEX_POINT('',#22867);
#6966=VERTEX_POINT('',#22871);
#6967=VERTEX_POINT('',#22878);
#6968=VERTEX_POINT('',#22879);
#6969=VERTEX_POINT('',#22883);
#6970=VERTEX_POINT('',#22890);
#6971=VERTEX_POINT('',#22915);
#6972=VERTEX_POINT('',#22917);
#6973=VERTEX_POINT('',#22919);
#6974=VERTEX_POINT('',#22923);
#6975=VERTEX_POINT('',#22924);
#6976=VERTEX_POINT('',#22929);
#6977=VERTEX_POINT('',#22931);
#6978=VERTEX_POINT('',#22937);
#6979=VERTEX_POINT('',#22938);
#6980=VERTEX_POINT('',#22940);
#6981=VERTEX_POINT('',#22944);
#6982=VERTEX_POINT('',#22948);
#6983=VERTEX_POINT('',#22950);
#6984=VERTEX_POINT('',#22958);
#6985=VERTEX_POINT('',#22962);
#6986=VERTEX_POINT('',#22966);
#6987=VERTEX_POINT('',#22968);
#6988=VERTEX_POINT('',#22976);
#6989=VERTEX_POINT('',#22977);
#6990=VERTEX_POINT('',#22981);
#6991=VERTEX_POINT('',#22983);
#6992=VERTEX_POINT('',#22994);
#6993=VERTEX_POINT('',#22998);
#6994=VERTEX_POINT('',#23002);
#6995=VERTEX_POINT('',#23004);
#6996=VERTEX_POINT('',#23012);
#6997=VERTEX_POINT('',#23016);
#6998=VERTEX_POINT('',#23020);
#6999=VERTEX_POINT('',#23022);
#7000=VERTEX_POINT('',#23030);
#7001=VERTEX_POINT('',#23037);
#7002=VERTEX_POINT('',#23072);
#7003=VERTEX_POINT('',#23073);
#7004=VERTEX_POINT('',#23075);
#7005=VERTEX_POINT('',#23087);
#7006=VERTEX_POINT('',#23095);
#7007=VERTEX_POINT('',#23096);
#7008=VERTEX_POINT('',#23141);
#7009=VERTEX_POINT('',#23142);
#7010=VERTEX_POINT('',#23187);
#7011=VERTEX_POINT('',#23188);
#7012=VERTEX_POINT('',#23233);
#7013=VERTEX_POINT('',#23234);
#7014=VERTEX_POINT('',#23279);
#7015=VERTEX_POINT('',#23280);
#7016=VERTEX_POINT('',#23325);
#7017=VERTEX_POINT('',#23326);
#7018=VERTEX_POINT('',#23371);
#7019=VERTEX_POINT('',#23372);
#7020=VERTEX_POINT('',#23417);
#7021=VERTEX_POINT('',#23418);
#7022=VERTEX_POINT('',#23463);
#7023=VERTEX_POINT('',#23464);
#7024=VERTEX_POINT('',#23509);
#7025=VERTEX_POINT('',#23510);
#7026=VERTEX_POINT('',#23555);
#7027=VERTEX_POINT('',#23556);
#7028=VERTEX_POINT('',#23601);
#7029=VERTEX_POINT('',#23602);
#7030=VERTEX_POINT('',#23647);
#7031=VERTEX_POINT('',#23648);
#7032=VERTEX_POINT('',#23693);
#7033=VERTEX_POINT('',#23694);
#7034=VERTEX_POINT('',#23739);
#7035=VERTEX_POINT('',#23740);
#7036=VERTEX_POINT('',#23785);
#7037=VERTEX_POINT('',#23786);
#7038=VERTEX_POINT('',#23831);
#7039=VERTEX_POINT('',#23832);
#7040=VERTEX_POINT('',#23877);
#7041=VERTEX_POINT('',#23878);
#7042=VERTEX_POINT('',#23923);
#7043=VERTEX_POINT('',#23924);
#7044=VERTEX_POINT('',#23969);
#7045=VERTEX_POINT('',#23970);
#7046=VERTEX_POINT('',#24015);
#7047=VERTEX_POINT('',#24016);
#7048=VERTEX_POINT('',#24061);
#7049=VERTEX_POINT('',#24062);
#7050=VERTEX_POINT('',#24064);
#7051=VERTEX_POINT('',#24101);
#7052=VERTEX_POINT('',#24103);
#7053=VERTEX_POINT('',#24150);
#7054=VERTEX_POINT('',#24266);
#7055=VERTEX_POINT('',#24319);
#7056=VERTEX_POINT('',#24366);
#7057=VERTEX_POINT('',#24534);
#7058=VERTEX_POINT('',#24553);
#7059=VERTEX_POINT('',#24584);
#7060=VERTEX_POINT('',#24585);
#7061=VERTEX_POINT('',#24660);
#7062=VERTEX_POINT('',#24661);
#7063=VERTEX_POINT('',#24736);
#7064=VERTEX_POINT('',#24737);
#7065=VERTEX_POINT('',#24812);
#7066=VERTEX_POINT('',#24813);
#7067=VERTEX_POINT('',#24888);
#7068=VERTEX_POINT('',#24889);
#7069=VERTEX_POINT('',#24964);
#7070=VERTEX_POINT('',#24965);
#7071=VERTEX_POINT('',#25042);
#7072=VERTEX_POINT('',#25043);
#7073=VERTEX_POINT('',#25118);
#7074=VERTEX_POINT('',#25119);
#7075=VERTEX_POINT('',#25194);
#7076=VERTEX_POINT('',#25195);
#7077=VERTEX_POINT('',#25272);
#7078=VERTEX_POINT('',#25273);
#7079=VERTEX_POINT('',#25348);
#7080=VERTEX_POINT('',#25349);
#7081=VERTEX_POINT('',#25424);
#7082=VERTEX_POINT('',#25425);
#7083=VERTEX_POINT('',#25500);
#7084=VERTEX_POINT('',#25501);
#7085=VERTEX_POINT('',#25576);
#7086=VERTEX_POINT('',#25577);
#7087=VERTEX_POINT('',#25652);
#7088=VERTEX_POINT('',#25653);
#7089=VERTEX_POINT('',#25730);
#7090=VERTEX_POINT('',#25731);
#7091=VERTEX_POINT('',#25806);
#7092=VERTEX_POINT('',#25807);
#7093=VERTEX_POINT('',#25884);
#7094=VERTEX_POINT('',#25885);
#7095=VERTEX_POINT('',#25960);
#7096=VERTEX_POINT('',#25961);
#7097=VERTEX_POINT('',#26036);
#7098=VERTEX_POINT('',#26037);
#7099=VERTEX_POINT('',#26039);
#7100=VERTEX_POINT('',#26112);
#7101=VERTEX_POINT('',#26113);
#7102=VERTEX_POINT('',#26115);
#7103=VERTEX_POINT('',#26117);
#7104=VERTEX_POINT('',#26121);
#7105=VERTEX_POINT('',#26122);
#7106=VERTEX_POINT('',#26124);
#7107=VERTEX_POINT('',#26126);
#7108=VERTEX_POINT('',#26130);
#7109=VERTEX_POINT('',#26132);
#7110=VERTEX_POINT('',#26285);
#7111=VERTEX_POINT('',#26287);
#7112=VERTEX_POINT('',#26306);
#7113=VERTEX_POINT('',#26335);
#7114=VERTEX_POINT('',#26392);
#7115=VERTEX_POINT('',#26450);
#7116=VERTEX_POINT('',#26504);
#7117=VERTEX_POINT('',#26563);
#7118=VERTEX_POINT('',#26565);
#7119=VERTEX_POINT('',#28353);
#7120=VERTEX_POINT('',#28504);
#7121=VERTEX_POINT('',#28621);
#7122=VERTEX_POINT('',#28772);
#7123=VERTEX_POINT('',#29141);
#7124=VERTEX_POINT('',#29142);
#7125=VERTEX_POINT('',#29144);
#7126=VERTEX_POINT('',#29160);
#7127=VERTEX_POINT('',#29184);
#7128=VERTEX_POINT('',#29185);
#7129=VERTEX_POINT('',#29230);
#7130=VERTEX_POINT('',#29231);
#7131=VERTEX_POINT('',#29276);
#7132=VERTEX_POINT('',#29277);
#7133=VERTEX_POINT('',#29322);
#7134=VERTEX_POINT('',#29323);
#7135=VERTEX_POINT('',#29325);
#7136=VERTEX_POINT('',#29341);
#7137=VERTEX_POINT('',#29363);
#7138=VERTEX_POINT('',#29364);
#7139=VERTEX_POINT('',#29366);
#7140=VERTEX_POINT('',#29377);
#7141=VERTEX_POINT('',#29378);
#7142=VERTEX_POINT('',#29380);
#7143=VERTEX_POINT('',#29455);
#7144=VERTEX_POINT('',#29456);
#7145=VERTEX_POINT('',#29531);
#7146=VERTEX_POINT('',#29532);
#7147=VERTEX_POINT('',#29607);
#7148=VERTEX_POINT('',#29608);
#7149=VERTEX_POINT('',#29683);
#7150=VERTEX_POINT('',#29684);
#7151=VERTEX_POINT('',#29686);
#7152=VERTEX_POINT('',#29705);
#7153=VERTEX_POINT('',#29730);
#7154=VERTEX_POINT('',#29732);
#7155=VERTEX_POINT('',#29736);
#7156=VERTEX_POINT('',#29737);
#7157=VERTEX_POINT('',#29742);
#7158=VERTEX_POINT('',#29744);
#7159=VERTEX_POINT('',#29746);
#7160=VERTEX_POINT('',#29748);
#7161=VERTEX_POINT('',#29756);
#7162=VERTEX_POINT('',#29760);
#7163=VERTEX_POINT('',#29768);
#7164=VERTEX_POINT('',#29845);
#7165=VERTEX_POINT('',#29851);
#7166=VERTEX_POINT('',#29853);
#7167=VERTEX_POINT('',#29855);
#7168=VERTEX_POINT('',#29859);
#7169=VERTEX_POINT('',#29861);
#7170=VERTEX_POINT('',#29865);
#7171=VERTEX_POINT('',#29867);
#7172=VERTEX_POINT('',#29873);
#7173=VERTEX_POINT('',#29879);
#7174=VERTEX_POINT('',#29883);
#7175=VERTEX_POINT('',#29885);
#7176=VERTEX_POINT('',#29889);
#7177=VERTEX_POINT('',#29891);
#7178=VERTEX_POINT('',#29898);
#7179=VERTEX_POINT('',#29900);
#7180=VERTEX_POINT('',#29902);
#7181=VERTEX_POINT('',#29904);
#7182=VERTEX_POINT('',#29906);
#7183=VERTEX_POINT('',#29908);
#7184=VERTEX_POINT('',#29910);
#7185=VERTEX_POINT('',#29912);
#7186=VERTEX_POINT('',#29952);
#7187=VERTEX_POINT('',#29954);
#7188=VERTEX_POINT('',#29956);
#7189=VERTEX_POINT('',#29958);
#7190=VERTEX_POINT('',#29960);
#7191=VERTEX_POINT('',#29962);
#7192=VERTEX_POINT('',#29964);
#7193=VERTEX_POINT('',#29966);
#7194=VERTEX_POINT('',#30005);
#7195=VERTEX_POINT('',#30006);
#7196=VERTEX_POINT('',#30021);
#7197=VERTEX_POINT('',#30022);
#7198=VERTEX_POINT('',#30037);
#7199=VERTEX_POINT('',#30038);
#7200=VERTEX_POINT('',#30672);
#7201=VERTEX_POINT('',#30674);
#7202=VERTEX_POINT('',#30678);
#7203=VERTEX_POINT('',#30680);
#7204=VERTEX_POINT('',#30707);
#7205=VERTEX_POINT('',#30708);
#7206=VERTEX_POINT('',#30710);
#7207=VERTEX_POINT('',#30712);
#7208=VERTEX_POINT('',#30716);
#7209=VERTEX_POINT('',#30718);
#7210=VERTEX_POINT('',#30722);
#7211=VERTEX_POINT('',#30724);
#7212=VERTEX_POINT('',#30733);
#7213=VERTEX_POINT('',#30735);
#7214=VERTEX_POINT('',#30739);
#7215=VERTEX_POINT('',#30740);
#7216=VERTEX_POINT('',#30742);
#7217=VERTEX_POINT('',#30744);
#7218=VERTEX_POINT('',#30746);
#7219=VERTEX_POINT('',#30748);
#7220=VERTEX_POINT('',#30752);
#7221=VERTEX_POINT('',#30753);
#7222=VERTEX_POINT('',#30755);
#7223=VERTEX_POINT('',#30757);
#7224=VERTEX_POINT('',#30759);
#7225=VERTEX_POINT('',#30761);
#7226=VERTEX_POINT('',#30777);
#7227=VERTEX_POINT('',#30779);
#7228=VERTEX_POINT('',#30783);
#7229=VERTEX_POINT('',#30784);
#7230=VERTEX_POINT('',#30786);
#7231=VERTEX_POINT('',#30788);
#7232=VERTEX_POINT('',#30790);
#7233=VERTEX_POINT('',#30792);
#7234=VERTEX_POINT('',#30796);
#7235=VERTEX_POINT('',#30797);
#7236=VERTEX_POINT('',#30799);
#7237=VERTEX_POINT('',#30801);
#7238=VERTEX_POINT('',#30803);
#7239=VERTEX_POINT('',#30805);
#7240=VERTEX_POINT('',#30821);
#7241=VERTEX_POINT('',#30823);
#7242=VERTEX_POINT('',#30827);
#7243=VERTEX_POINT('',#30829);
#7244=VERTEX_POINT('',#30833);
#7245=VERTEX_POINT('',#30835);
#7246=VERTEX_POINT('',#30839);
#7247=VERTEX_POINT('',#30841);
#7248=VERTEX_POINT('',#30845);
#7249=VERTEX_POINT('',#30847);
#7250=VERTEX_POINT('',#30851);
#7251=VERTEX_POINT('',#30852);
#7252=VERTEX_POINT('',#30854);
#7253=VERTEX_POINT('',#30856);
#7254=VERTEX_POINT('',#30858);
#7255=VERTEX_POINT('',#30860);
#7256=VERTEX_POINT('',#30862);
#7257=VERTEX_POINT('',#30864);
#7258=VERTEX_POINT('',#30868);
#7259=VERTEX_POINT('',#30869);
#7260=VERTEX_POINT('',#30871);
#7261=VERTEX_POINT('',#30873);
#7262=VERTEX_POINT('',#30875);
#7263=VERTEX_POINT('',#30877);
#7264=VERTEX_POINT('',#30879);
#7265=VERTEX_POINT('',#30881);
#7266=VERTEX_POINT('',#30901);
#7267=VERTEX_POINT('',#30902);
#7268=VERTEX_POINT('',#30904);
#7269=VERTEX_POINT('',#30906);
#7270=VERTEX_POINT('',#30910);
#7271=VERTEX_POINT('',#30912);
#7272=VERTEX_POINT('',#30916);
#7273=VERTEX_POINT('',#30918);
#7274=VERTEX_POINT('',#30927);
#7275=VERTEX_POINT('',#30928);
#7276=VERTEX_POINT('',#30930);
#7277=VERTEX_POINT('',#30932);
#7278=VERTEX_POINT('',#30936);
#7279=VERTEX_POINT('',#30938);
#7280=VERTEX_POINT('',#30942);
#7281=VERTEX_POINT('',#30944);
#7282=VERTEX_POINT('',#30953);
#7283=VERTEX_POINT('',#30954);
#7284=VERTEX_POINT('',#30956);
#7285=VERTEX_POINT('',#30958);
#7286=VERTEX_POINT('',#30962);
#7287=VERTEX_POINT('',#30964);
#7288=VERTEX_POINT('',#30968);
#7289=VERTEX_POINT('',#30970);
#7290=VERTEX_POINT('',#30974);
#7291=VERTEX_POINT('',#30976);
#7292=VERTEX_POINT('',#30980);
#7293=VERTEX_POINT('',#30982);
#7294=VERTEX_POINT('',#30991);
#7295=VERTEX_POINT('',#30993);
#7296=VERTEX_POINT('',#30997);
#7297=VERTEX_POINT('',#30999);
#7298=VERTEX_POINT('',#31003);
#7299=VERTEX_POINT('',#31005);
#7300=VERTEX_POINT('',#31009);
#7301=VERTEX_POINT('',#31010);
#7302=VERTEX_POINT('',#31012);
#7303=VERTEX_POINT('',#31014);
#7304=VERTEX_POINT('',#31018);
#7305=VERTEX_POINT('',#31019);
#7306=VERTEX_POINT('',#31021);
#7307=VERTEX_POINT('',#31023);
#7308=VERTEX_POINT('',#31035);
#7309=VERTEX_POINT('',#31037);
#7310=VERTEX_POINT('',#31041);
#7311=VERTEX_POINT('',#31043);
#7312=VERTEX_POINT('',#31047);
#7313=VERTEX_POINT('',#31049);
#7314=VERTEX_POINT('',#31053);
#7315=VERTEX_POINT('',#31054);
#7316=VERTEX_POINT('',#31056);
#7317=VERTEX_POINT('',#31058);
#7318=VERTEX_POINT('',#31062);
#7319=VERTEX_POINT('',#31063);
#7320=VERTEX_POINT('',#31065);
#7321=VERTEX_POINT('',#31067);
#7322=VERTEX_POINT('',#31079);
#7323=VERTEX_POINT('',#31081);
#7324=VERTEX_POINT('',#31085);
#7325=VERTEX_POINT('',#31087);
#7326=VERTEX_POINT('',#31091);
#7327=VERTEX_POINT('',#31093);
#7328=VERTEX_POINT('',#31097);
#7329=VERTEX_POINT('',#31098);
#7330=VERTEX_POINT('',#31100);
#7331=VERTEX_POINT('',#31102);
#7332=VERTEX_POINT('',#31106);
#7333=VERTEX_POINT('',#31107);
#7334=VERTEX_POINT('',#31109);
#7335=VERTEX_POINT('',#31111);
#7336=VERTEX_POINT('',#31123);
#7337=VERTEX_POINT('',#31125);
#7338=VERTEX_POINT('',#31129);
#7339=VERTEX_POINT('',#31131);
#7340=VERTEX_POINT('',#31135);
#7341=VERTEX_POINT('',#31137);
#7342=VERTEX_POINT('',#31141);
#7343=VERTEX_POINT('',#31142);
#7344=VERTEX_POINT('',#31144);
#7345=VERTEX_POINT('',#31146);
#7346=VERTEX_POINT('',#31150);
#7347=VERTEX_POINT('',#31151);
#7348=VERTEX_POINT('',#31153);
#7349=VERTEX_POINT('',#31155);
#7350=VERTEX_POINT('',#31167);
#7351=VERTEX_POINT('',#31168);
#7352=VERTEX_POINT('',#31170);
#7353=VERTEX_POINT('',#31172);
#7354=VERTEX_POINT('',#31176);
#7355=VERTEX_POINT('',#31178);
#7356=VERTEX_POINT('',#31182);
#7357=VERTEX_POINT('',#31184);
#7358=VERTEX_POINT('',#31193);
#7359=VERTEX_POINT('',#31194);
#7360=VERTEX_POINT('',#31196);
#7361=VERTEX_POINT('',#31198);
#7362=VERTEX_POINT('',#31202);
#7363=VERTEX_POINT('',#31204);
#7364=VERTEX_POINT('',#31208);
#7365=VERTEX_POINT('',#31210);
#7366=VERTEX_POINT('',#31219);
#7367=VERTEX_POINT('',#31220);
#7368=VERTEX_POINT('',#31222);
#7369=VERTEX_POINT('',#31224);
#7370=VERTEX_POINT('',#31228);
#7371=VERTEX_POINT('',#31230);
#7372=VERTEX_POINT('',#31234);
#7373=VERTEX_POINT('',#31236);
#7374=VERTEX_POINT('',#31245);
#7375=VERTEX_POINT('',#31246);
#7376=VERTEX_POINT('',#31248);
#7377=VERTEX_POINT('',#31250);
#7378=VERTEX_POINT('',#31254);
#7379=VERTEX_POINT('',#31256);
#7380=VERTEX_POINT('',#31260);
#7381=VERTEX_POINT('',#31262);
#7382=VERTEX_POINT('',#31271);
#7383=VERTEX_POINT('',#31272);
#7384=VERTEX_POINT('',#31274);
#7385=VERTEX_POINT('',#31276);
#7386=VERTEX_POINT('',#31280);
#7387=VERTEX_POINT('',#31282);
#7388=VERTEX_POINT('',#31286);
#7389=VERTEX_POINT('',#31288);
#7390=VERTEX_POINT('',#31297);
#7391=VERTEX_POINT('',#31299);
#7392=VERTEX_POINT('',#31303);
#7393=VERTEX_POINT('',#31305);
#7394=VERTEX_POINT('',#31309);
#7395=VERTEX_POINT('',#31311);
#7396=VERTEX_POINT('',#31315);
#7397=VERTEX_POINT('',#31317);
#7398=VERTEX_POINT('',#31321);
#7399=VERTEX_POINT('',#31322);
#7400=VERTEX_POINT('',#31324);
#7401=VERTEX_POINT('',#31326);
#7402=VERTEX_POINT('',#31330);
#7403=VERTEX_POINT('',#31331);
#7404=VERTEX_POINT('',#31333);
#7405=VERTEX_POINT('',#31335);
#7406=VERTEX_POINT('',#31347);
#7407=VERTEX_POINT('',#31349);
#7408=VERTEX_POINT('',#31353);
#7409=VERTEX_POINT('',#31355);
#7410=VERTEX_POINT('',#31359);
#7411=VERTEX_POINT('',#31361);
#7412=VERTEX_POINT('',#31365);
#7413=VERTEX_POINT('',#31367);
#7414=VERTEX_POINT('',#31371);
#7415=VERTEX_POINT('',#31373);
#7416=VERTEX_POINT('',#31377);
#7417=VERTEX_POINT('',#31379);
#7418=VERTEX_POINT('',#31383);
#7419=VERTEX_POINT('',#31384);
#7420=VERTEX_POINT('',#31386);
#7421=VERTEX_POINT('',#31388);
#7422=VERTEX_POINT('',#31392);
#7423=VERTEX_POINT('',#31394);
#7424=VERTEX_POINT('',#31398);
#7425=VERTEX_POINT('',#31400);
#7426=VERTEX_POINT('',#31409);
#7427=VERTEX_POINT('',#31410);
#7428=VERTEX_POINT('',#31412);
#7429=VERTEX_POINT('',#31414);
#7430=VERTEX_POINT('',#31418);
#7431=VERTEX_POINT('',#31420);
#7432=VERTEX_POINT('',#31424);
#7433=VERTEX_POINT('',#31426);
#7434=VERTEX_POINT('',#31430);
#7435=VERTEX_POINT('',#31432);
#7436=VERTEX_POINT('',#31436);
#7437=VERTEX_POINT('',#31438);
#7438=VERTEX_POINT('',#31442);
#7439=VERTEX_POINT('',#31444);
#7440=VERTEX_POINT('',#31453);
#7441=VERTEX_POINT('',#31454);
#7442=VERTEX_POINT('',#31456);
#7443=VERTEX_POINT('',#31458);
#7444=VERTEX_POINT('',#31462);
#7445=VERTEX_POINT('',#31464);
#7446=VERTEX_POINT('',#31468);
#7447=VERTEX_POINT('',#31470);
#7448=VERTEX_POINT('',#31474);
#7449=VERTEX_POINT('',#31476);
#7450=VERTEX_POINT('',#31480);
#7451=VERTEX_POINT('',#31482);
#7452=VERTEX_POINT('',#31486);
#7453=VERTEX_POINT('',#31488);
#7454=VERTEX_POINT('',#31497);
#7455=VERTEX_POINT('',#31498);
#7456=VERTEX_POINT('',#31500);
#7457=VERTEX_POINT('',#31502);
#7458=VERTEX_POINT('',#31506);
#7459=VERTEX_POINT('',#31508);
#7460=VERTEX_POINT('',#31512);
#7461=VERTEX_POINT('',#31514);
#7462=VERTEX_POINT('',#31518);
#7463=VERTEX_POINT('',#31520);
#7464=VERTEX_POINT('',#31524);
#7465=VERTEX_POINT('',#31526);
#7466=VERTEX_POINT('',#31530);
#7467=VERTEX_POINT('',#31532);
#7468=VERTEX_POINT('',#31541);
#7469=VERTEX_POINT('',#31542);
#7470=VERTEX_POINT('',#31544);
#7471=VERTEX_POINT('',#31546);
#7472=VERTEX_POINT('',#31550);
#7473=VERTEX_POINT('',#31552);
#7474=VERTEX_POINT('',#31556);
#7475=VERTEX_POINT('',#31558);
#7476=VERTEX_POINT('',#31562);
#7477=VERTEX_POINT('',#31564);
#7478=VERTEX_POINT('',#31568);
#7479=VERTEX_POINT('',#31570);
#7480=VERTEX_POINT('',#31574);
#7481=VERTEX_POINT('',#31576);
#7482=VERTEX_POINT('',#31585);
#7483=VERTEX_POINT('',#31586);
#7484=VERTEX_POINT('',#31588);
#7485=VERTEX_POINT('',#31590);
#7486=VERTEX_POINT('',#31594);
#7487=VERTEX_POINT('',#31596);
#7488=VERTEX_POINT('',#31600);
#7489=VERTEX_POINT('',#31602);
#7490=VERTEX_POINT('',#31606);
#7491=VERTEX_POINT('',#31608);
#7492=VERTEX_POINT('',#31612);
#7493=VERTEX_POINT('',#31614);
#7494=VERTEX_POINT('',#31618);
#7495=VERTEX_POINT('',#31620);
#7496=VERTEX_POINT('',#31629);
#7497=VERTEX_POINT('',#31630);
#7498=VERTEX_POINT('',#31632);
#7499=VERTEX_POINT('',#31634);
#7500=VERTEX_POINT('',#31638);
#7501=VERTEX_POINT('',#31640);
#7502=VERTEX_POINT('',#31644);
#7503=VERTEX_POINT('',#31646);
#7504=VERTEX_POINT('',#31650);
#7505=VERTEX_POINT('',#31652);
#7506=VERTEX_POINT('',#31656);
#7507=VERTEX_POINT('',#31658);
#7508=VERTEX_POINT('',#31662);
#7509=VERTEX_POINT('',#31664);
#7510=VERTEX_POINT('',#31673);
#7511=VERTEX_POINT('',#31674);
#7512=VERTEX_POINT('',#31676);
#7513=VERTEX_POINT('',#31678);
#7514=VERTEX_POINT('',#31682);
#7515=VERTEX_POINT('',#31684);
#7516=VERTEX_POINT('',#31688);
#7517=VERTEX_POINT('',#31690);
#7518=VERTEX_POINT('',#31694);
#7519=VERTEX_POINT('',#31696);
#7520=VERTEX_POINT('',#31700);
#7521=VERTEX_POINT('',#31702);
#7522=VERTEX_POINT('',#31706);
#7523=VERTEX_POINT('',#31708);
#7524=VERTEX_POINT('',#31717);
#7525=VERTEX_POINT('',#31718);
#7526=VERTEX_POINT('',#31720);
#7527=VERTEX_POINT('',#31722);
#7528=VERTEX_POINT('',#31726);
#7529=VERTEX_POINT('',#31728);
#7530=VERTEX_POINT('',#31732);
#7531=VERTEX_POINT('',#31734);
#7532=VERTEX_POINT('',#31738);
#7533=VERTEX_POINT('',#31740);
#7534=VERTEX_POINT('',#31744);
#7535=VERTEX_POINT('',#31746);
#7536=VERTEX_POINT('',#31750);
#7537=VERTEX_POINT('',#31752);
#7538=VERTEX_POINT('',#31761);
#7539=VERTEX_POINT('',#31762);
#7540=VERTEX_POINT('',#31764);
#7541=VERTEX_POINT('',#31766);
#7542=VERTEX_POINT('',#31770);
#7543=VERTEX_POINT('',#31772);
#7544=VERTEX_POINT('',#31776);
#7545=VERTEX_POINT('',#31778);
#7546=VERTEX_POINT('',#31782);
#7547=VERTEX_POINT('',#31784);
#7548=VERTEX_POINT('',#31788);
#7549=VERTEX_POINT('',#31790);
#7550=VERTEX_POINT('',#31794);
#7551=VERTEX_POINT('',#31796);
#7552=VERTEX_POINT('',#31805);
#7553=VERTEX_POINT('',#31806);
#7554=VERTEX_POINT('',#31808);
#7555=VERTEX_POINT('',#31810);
#7556=VERTEX_POINT('',#31814);
#7557=VERTEX_POINT('',#31816);
#7558=VERTEX_POINT('',#31820);
#7559=VERTEX_POINT('',#31822);
#7560=VERTEX_POINT('',#31826);
#7561=VERTEX_POINT('',#31828);
#7562=VERTEX_POINT('',#31832);
#7563=VERTEX_POINT('',#31834);
#7564=VERTEX_POINT('',#31838);
#7565=VERTEX_POINT('',#31840);
#7566=VERTEX_POINT('',#31849);
#7567=VERTEX_POINT('',#31850);
#7568=VERTEX_POINT('',#31852);
#7569=VERTEX_POINT('',#31854);
#7570=VERTEX_POINT('',#31858);
#7571=VERTEX_POINT('',#31860);
#7572=VERTEX_POINT('',#31864);
#7573=VERTEX_POINT('',#31866);
#7574=VERTEX_POINT('',#31870);
#7575=VERTEX_POINT('',#31872);
#7576=VERTEX_POINT('',#31876);
#7577=VERTEX_POINT('',#31878);
#7578=VERTEX_POINT('',#31882);
#7579=VERTEX_POINT('',#31884);
#7580=VERTEX_POINT('',#31893);
#7581=VERTEX_POINT('',#31895);
#7582=VERTEX_POINT('',#31899);
#7583=VERTEX_POINT('',#31901);
#7584=VERTEX_POINT('',#31905);
#7585=VERTEX_POINT('',#31907);
#7586=VERTEX_POINT('',#31911);
#7587=VERTEX_POINT('',#31913);
#7588=VERTEX_POINT('',#31917);
#7589=VERTEX_POINT('',#31918);
#7590=VERTEX_POINT('',#31920);
#7591=VERTEX_POINT('',#31922);
#7592=VERTEX_POINT('',#31926);
#7593=VERTEX_POINT('',#31927);
#7594=VERTEX_POINT('',#31929);
#7595=VERTEX_POINT('',#31931);
#7596=VERTEX_POINT('',#31943);
#7597=VERTEX_POINT('',#31944);
#7598=VERTEX_POINT('',#31946);
#7599=VERTEX_POINT('',#31948);
#7600=VERTEX_POINT('',#31952);
#7601=VERTEX_POINT('',#31954);
#7602=VERTEX_POINT('',#31958);
#7603=VERTEX_POINT('',#31960);
#7604=VERTEX_POINT('',#31969);
#7605=VERTEX_POINT('',#31970);
#7606=VERTEX_POINT('',#31972);
#7607=VERTEX_POINT('',#31974);
#7608=VERTEX_POINT('',#31978);
#7609=VERTEX_POINT('',#31980);
#7610=VERTEX_POINT('',#31984);
#7611=VERTEX_POINT('',#31986);
#7612=VERTEX_POINT('',#31995);
#7613=VERTEX_POINT('',#31996);
#7614=VERTEX_POINT('',#31998);
#7615=VERTEX_POINT('',#32000);
#7616=VERTEX_POINT('',#32004);
#7617=VERTEX_POINT('',#32006);
#7618=VERTEX_POINT('',#32010);
#7619=VERTEX_POINT('',#32012);
#7620=VERTEX_POINT('',#32021);
#7621=VERTEX_POINT('',#32022);
#7622=VERTEX_POINT('',#32024);
#7623=VERTEX_POINT('',#32026);
#7624=VERTEX_POINT('',#32030);
#7625=VERTEX_POINT('',#32032);
#7626=VERTEX_POINT('',#32036);
#7627=VERTEX_POINT('',#32038);
#7628=VERTEX_POINT('',#32047);
#7629=VERTEX_POINT('',#32048);
#7630=VERTEX_POINT('',#32050);
#7631=VERTEX_POINT('',#32052);
#7632=VERTEX_POINT('',#32056);
#7633=VERTEX_POINT('',#32058);
#7634=VERTEX_POINT('',#32062);
#7635=VERTEX_POINT('',#32064);
#7636=VERTEX_POINT('',#32073);
#7637=VERTEX_POINT('',#32074);
#7638=VERTEX_POINT('',#32076);
#7639=VERTEX_POINT('',#32078);
#7640=VERTEX_POINT('',#32082);
#7641=VERTEX_POINT('',#32084);
#7642=VERTEX_POINT('',#32088);
#7643=VERTEX_POINT('',#32090);
#7644=VERTEX_POINT('',#32099);
#7645=VERTEX_POINT('',#32100);
#7646=VERTEX_POINT('',#32102);
#7647=VERTEX_POINT('',#32104);
#7648=VERTEX_POINT('',#32108);
#7649=VERTEX_POINT('',#32110);
#7650=VERTEX_POINT('',#32114);
#7651=VERTEX_POINT('',#32116);
#7652=VERTEX_POINT('',#32125);
#7653=VERTEX_POINT('',#32126);
#7654=VERTEX_POINT('',#32128);
#7655=VERTEX_POINT('',#32130);
#7656=VERTEX_POINT('',#32134);
#7657=VERTEX_POINT('',#32136);
#7658=VERTEX_POINT('',#32140);
#7659=VERTEX_POINT('',#32142);
#7660=VERTEX_POINT('',#32151);
#7661=VERTEX_POINT('',#32152);
#7662=VERTEX_POINT('',#32154);
#7663=VERTEX_POINT('',#32156);
#7664=VERTEX_POINT('',#32160);
#7665=VERTEX_POINT('',#32162);
#7666=VERTEX_POINT('',#32166);
#7667=VERTEX_POINT('',#32168);
#7668=VERTEX_POINT('',#32177);
#7669=VERTEX_POINT('',#32178);
#7670=VERTEX_POINT('',#32180);
#7671=VERTEX_POINT('',#32182);
#7672=VERTEX_POINT('',#32186);
#7673=VERTEX_POINT('',#32188);
#7674=VERTEX_POINT('',#32192);
#7675=VERTEX_POINT('',#32194);
#7676=VERTEX_POINT('',#32203);
#7677=VERTEX_POINT('',#32204);
#7678=VERTEX_POINT('',#32206);
#7679=VERTEX_POINT('',#32208);
#7680=VERTEX_POINT('',#32212);
#7681=VERTEX_POINT('',#32214);
#7682=VERTEX_POINT('',#32218);
#7683=VERTEX_POINT('',#32220);
#7684=VERTEX_POINT('',#32229);
#7685=VERTEX_POINT('',#32230);
#7686=VERTEX_POINT('',#32232);
#7687=VERTEX_POINT('',#32234);
#7688=VERTEX_POINT('',#32238);
#7689=VERTEX_POINT('',#32240);
#7690=VERTEX_POINT('',#32244);
#7691=VERTEX_POINT('',#32246);
#7692=VERTEX_POINT('',#32255);
#7693=VERTEX_POINT('',#32256);
#7694=VERTEX_POINT('',#32258);
#7695=VERTEX_POINT('',#32260);
#7696=VERTEX_POINT('',#32264);
#7697=VERTEX_POINT('',#32266);
#7698=VERTEX_POINT('',#32270);
#7699=VERTEX_POINT('',#32272);
#7700=VERTEX_POINT('',#32281);
#7701=VERTEX_POINT('',#32282);
#7702=VERTEX_POINT('',#32284);
#7703=VERTEX_POINT('',#32286);
#7704=VERTEX_POINT('',#32290);
#7705=VERTEX_POINT('',#32292);
#7706=VERTEX_POINT('',#32296);
#7707=VERTEX_POINT('',#32298);
#7708=VERTEX_POINT('',#32307);
#7709=VERTEX_POINT('',#32308);
#7710=VERTEX_POINT('',#32310);
#7711=VERTEX_POINT('',#32312);
#7712=VERTEX_POINT('',#32316);
#7713=VERTEX_POINT('',#32318);
#7714=VERTEX_POINT('',#32322);
#7715=VERTEX_POINT('',#32324);
#7716=VERTEX_POINT('',#32333);
#7717=VERTEX_POINT('',#32334);
#7718=VERTEX_POINT('',#32336);
#7719=VERTEX_POINT('',#32338);
#7720=VERTEX_POINT('',#32342);
#7721=VERTEX_POINT('',#32344);
#7722=VERTEX_POINT('',#32348);
#7723=VERTEX_POINT('',#32350);
#7724=VERTEX_POINT('',#32359);
#7725=VERTEX_POINT('',#32360);
#7726=VERTEX_POINT('',#32362);
#7727=VERTEX_POINT('',#32364);
#7728=VERTEX_POINT('',#32368);
#7729=VERTEX_POINT('',#32370);
#7730=VERTEX_POINT('',#32374);
#7731=VERTEX_POINT('',#32376);
#7732=VERTEX_POINT('',#32385);
#7733=VERTEX_POINT('',#32386);
#7734=VERTEX_POINT('',#32388);
#7735=VERTEX_POINT('',#32390);
#7736=VERTEX_POINT('',#32394);
#7737=VERTEX_POINT('',#32396);
#7738=VERTEX_POINT('',#32400);
#7739=VERTEX_POINT('',#32402);
#7740=VERTEX_POINT('',#32411);
#7741=VERTEX_POINT('',#32412);
#7742=VERTEX_POINT('',#32414);
#7743=VERTEX_POINT('',#32416);
#7744=VERTEX_POINT('',#32420);
#7745=VERTEX_POINT('',#32422);
#7746=VERTEX_POINT('',#32426);
#7747=VERTEX_POINT('',#32428);
#7748=VERTEX_POINT('',#32437);
#7749=VERTEX_POINT('',#32438);
#7750=VERTEX_POINT('',#32440);
#7751=VERTEX_POINT('',#32442);
#7752=VERTEX_POINT('',#32446);
#7753=VERTEX_POINT('',#32448);
#7754=VERTEX_POINT('',#32452);
#7755=VERTEX_POINT('',#32454);
#7756=VERTEX_POINT('',#32463);
#7757=VERTEX_POINT('',#32464);
#7758=VERTEX_POINT('',#32466);
#7759=VERTEX_POINT('',#32468);
#7760=VERTEX_POINT('',#32472);
#7761=VERTEX_POINT('',#32474);
#7762=VERTEX_POINT('',#32478);
#7763=VERTEX_POINT('',#32480);
#7764=VERTEX_POINT('',#32489);
#7765=VERTEX_POINT('',#32490);
#7766=VERTEX_POINT('',#32492);
#7767=VERTEX_POINT('',#32494);
#7768=VERTEX_POINT('',#32498);
#7769=VERTEX_POINT('',#32500);
#7770=VERTEX_POINT('',#32504);
#7771=VERTEX_POINT('',#32506);
#7772=VERTEX_POINT('',#32516);
#7773=VERTEX_POINT('',#32517);
#7774=VERTEX_POINT('',#32520);
#7775=VERTEX_POINT('',#32524);
#7776=VERTEX_POINT('',#32525);
#7777=VERTEX_POINT('',#32527);
#7778=VERTEX_POINT('',#32529);
#7779=VERTEX_POINT('',#32531);
#7780=VERTEX_POINT('',#32534);
#7781=VERTEX_POINT('',#32536);
#7782=VERTEX_POINT('',#32540);
#7783=VERTEX_POINT('',#32542);
#7784=VERTEX_POINT('',#32550);
#7785=VERTEX_POINT('',#32554);
#7786=VERTEX_POINT('',#32558);
#7787=VERTEX_POINT('',#32562);
#7788=VERTEX_POINT('',#32566);
#7789=VERTEX_POINT('',#32570);
#7790=VERTEX_POINT('',#32574);
#7791=VERTEX_POINT('',#32575);
#7792=VERTEX_POINT('',#32577);
#7793=VERTEX_POINT('',#32579);
#7794=VERTEX_POINT('',#32581);
#7795=VERTEX_POINT('',#32583);
#7796=VERTEX_POINT('',#32587);
#7797=VERTEX_POINT('',#32595);
#7798=VERTEX_POINT('',#32603);
#7799=VERTEX_POINT('',#32611);
#7800=VERTEX_POINT('',#32619);
#7801=VERTEX_POINT('',#32627);
#7802=VERTEX_POINT('',#32648);
#7803=VERTEX_POINT('',#32650);
#7804=VERTEX_POINT('',#32654);
#7805=VERTEX_POINT('',#32656);
#7806=VERTEX_POINT('',#32663);
#7807=VERTEX_POINT('',#32665);
#7808=VERTEX_POINT('',#32667);
#7809=VERTEX_POINT('',#32671);
#7810=VERTEX_POINT('',#32672);
#7811=VERTEX_POINT('',#32677);
#7812=VERTEX_POINT('',#32679);
#7813=VERTEX_POINT('',#32685);
#7814=VERTEX_POINT('',#32686);
#7815=VERTEX_POINT('',#32688);
#7816=VERTEX_POINT('',#32692);
#7817=VERTEX_POINT('',#32696);
#7818=VERTEX_POINT('',#32698);
#7819=VERTEX_POINT('',#32706);
#7820=VERTEX_POINT('',#32710);
#7821=VERTEX_POINT('',#32714);
#7822=VERTEX_POINT('',#32716);
#7823=VERTEX_POINT('',#32724);
#7824=VERTEX_POINT('',#32725);
#7825=VERTEX_POINT('',#32729);
#7826=VERTEX_POINT('',#32731);
#7827=VERTEX_POINT('',#32742);
#7828=VERTEX_POINT('',#32746);
#7829=VERTEX_POINT('',#32750);
#7830=VERTEX_POINT('',#32752);
#7831=VERTEX_POINT('',#32760);
#7832=VERTEX_POINT('',#32764);
#7833=VERTEX_POINT('',#32768);
#7834=VERTEX_POINT('',#32770);
#7835=VERTEX_POINT('',#32778);
#7836=VERTEX_POINT('',#32785);
#7837=EDGE_CURVE('',#6481,#6482,#3673,.T.);
#7838=EDGE_CURVE('',#6483,#6481,#3674,.T.);
#7839=EDGE_CURVE('',#6483,#6484,#3675,.T.);
#7840=EDGE_CURVE('',#6484,#6482,#3676,.T.);
#7841=EDGE_CURVE('',#6485,#6481,#3677,.T.);
#7842=EDGE_CURVE('',#6486,#6485,#3678,.T.);
#7843=EDGE_CURVE('',#6486,#6483,#3679,.T.);
#7844=EDGE_CURVE('',#6487,#6485,#3680,.T.);
#7845=EDGE_CURVE('',#6488,#6487,#3681,.T.);
#7846=EDGE_CURVE('',#6488,#6486,#3682,.T.);
#7847=EDGE_CURVE('',#6482,#6487,#3683,.T.);
#7848=EDGE_CURVE('',#6484,#6488,#3684,.T.);
#7849=EDGE_CURVE('',#6489,#6490,#3685,.T.);
#7850=EDGE_CURVE('',#6490,#6491,#3686,.T.);
#7851=EDGE_CURVE('',#6491,#6492,#3687,.T.);
#7852=EDGE_CURVE('',#6492,#6489,#3688,.T.);
#7853=EDGE_CURVE('',#6493,#6494,#3689,.T.);
#7854=EDGE_CURVE('',#6495,#6493,#3690,.T.);
#7855=EDGE_CURVE('',#6496,#6495,#3691,.T.);
#7856=EDGE_CURVE('',#6494,#6496,#3692,.T.);
#7857=EDGE_CURVE('',#6490,#6493,#3693,.T.);
#7858=EDGE_CURVE('',#6489,#6495,#3694,.T.);
#7859=EDGE_CURVE('',#6492,#6496,#3695,.T.);
#7860=EDGE_CURVE('',#6491,#6494,#3696,.T.);
#7861=EDGE_CURVE('',#6497,#6498,#3697,.T.);
#7862=EDGE_CURVE('',#6499,#6498,#3698,.T.);
#7863=EDGE_CURVE('',#6500,#6499,#3699,.T.);
#7864=EDGE_CURVE('',#6500,#6497,#3700,.T.);
#7865=EDGE_CURVE('',#6498,#6501,#3701,.T.);
#7866=EDGE_CURVE('',#6502,#6501,#3702,.T.);
#7867=EDGE_CURVE('',#6499,#6502,#3703,.T.);
#7868=EDGE_CURVE('',#6501,#6503,#700,.T.);
#7869=EDGE_CURVE('',#6504,#6503,#3704,.T.);
#7870=EDGE_CURVE('',#6502,#6504,#701,.T.);
#7871=EDGE_CURVE('',#6503,#6505,#3705,.T.);
#7872=EDGE_CURVE('',#6506,#6505,#3706,.T.);
#7873=EDGE_CURVE('',#6504,#6506,#3707,.T.);
#7874=EDGE_CURVE('',#6505,#6507,#3708,.T.);
#7875=EDGE_CURVE('',#6508,#6507,#3709,.T.);
#7876=EDGE_CURVE('',#6506,#6508,#3710,.T.);
#7877=EDGE_CURVE('',#6507,#6497,#3711,.T.);
#7878=EDGE_CURVE('',#6508,#6500,#3712,.T.);
#7879=EDGE_CURVE('',#6509,#6510,#3713,.T.);
#7880=EDGE_CURVE('',#6511,#6509,#3714,.T.);
#7881=EDGE_CURVE('',#6511,#6512,#3715,.T.);
#7882=EDGE_CURVE('',#6512,#6510,#3716,.T.);
#7883=EDGE_CURVE('',#6510,#6513,#3717,.T.);
#7884=EDGE_CURVE('',#6512,#6514,#3718,.T.);
#7885=EDGE_CURVE('',#6514,#6513,#3719,.T.);
#7886=EDGE_CURVE('',#6513,#6515,#702,.T.);
#7887=EDGE_CURVE('',#6514,#6516,#703,.T.);
#7888=EDGE_CURVE('',#6516,#6515,#3720,.T.);
#7889=EDGE_CURVE('',#6515,#6517,#3721,.T.);
#7890=EDGE_CURVE('',#6516,#6518,#3722,.T.);
#7891=EDGE_CURVE('',#6518,#6517,#3723,.T.);
#7892=EDGE_CURVE('',#6517,#6519,#3724,.T.);
#7893=EDGE_CURVE('',#6518,#6520,#3725,.T.);
#7894=EDGE_CURVE('',#6520,#6519,#3726,.T.);
#7895=EDGE_CURVE('',#6519,#6509,#3727,.T.);
#7896=EDGE_CURVE('',#6520,#6511,#3728,.T.);
#7897=EDGE_CURVE('',#6521,#6521,#704,.T.);
#7898=EDGE_CURVE('',#6521,#6522,#3729,.T.);
#7899=EDGE_CURVE('',#6522,#6522,#705,.T.);
#7900=EDGE_CURVE('',#6523,#6523,#706,.T.);
#7901=EDGE_CURVE('',#6523,#6524,#3730,.T.);
#7902=EDGE_CURVE('',#6524,#6524,#707,.T.);
#7903=EDGE_CURVE('',#6525,#6525,#708,.T.);
#7904=EDGE_CURVE('',#6525,#6526,#3731,.T.);
#7905=EDGE_CURVE('',#6526,#6526,#709,.T.);
#7906=EDGE_CURVE('',#6527,#6527,#710,.T.);
#7907=EDGE_CURVE('',#6527,#6528,#3732,.T.);
#7908=EDGE_CURVE('',#6528,#6528,#711,.T.);
#7909=EDGE_CURVE('',#6529,#6529,#712,.T.);
#7910=EDGE_CURVE('',#6529,#6530,#3733,.T.);
#7911=EDGE_CURVE('',#6530,#6530,#713,.T.);
#7912=EDGE_CURVE('',#6531,#6531,#714,.T.);
#7913=EDGE_CURVE('',#6531,#6532,#3734,.T.);
#7914=EDGE_CURVE('',#6532,#6532,#715,.T.);
#7915=EDGE_CURVE('',#6533,#6534,#3735,.T.);
#7916=EDGE_CURVE('',#6534,#6535,#3736,.T.);
#7917=EDGE_CURVE('',#6535,#6536,#3737,.T.);
#7918=EDGE_CURVE('',#6536,#6533,#3738,.T.);
#7919=EDGE_CURVE('',#6537,#6538,#3739,.T.);
#7920=EDGE_CURVE('',#6539,#6537,#3740,.T.);
#7921=EDGE_CURVE('',#6540,#6539,#3741,.T.);
#7922=EDGE_CURVE('',#6538,#6540,#3742,.T.);
#7923=EDGE_CURVE('',#6534,#6538,#3743,.T.);
#7924=EDGE_CURVE('',#6533,#6537,#3744,.T.);
#7925=EDGE_CURVE('',#6535,#6540,#3745,.T.);
#7926=EDGE_CURVE('',#6536,#6539,#3746,.T.);
#7927=EDGE_CURVE('',#6541,#6541,#716,.T.);
#7928=EDGE_CURVE('',#6541,#6542,#3747,.T.);
#7929=EDGE_CURVE('',#6542,#6542,#717,.T.);
#7930=EDGE_CURVE('',#6543,#6543,#718,.T.);
#7931=EDGE_CURVE('',#6543,#6544,#3748,.T.);
#7932=EDGE_CURVE('',#6544,#6544,#719,.T.);
#7933=EDGE_CURVE('',#6545,#6545,#720,.T.);
#7934=EDGE_CURVE('',#6545,#6546,#3749,.T.);
#7935=EDGE_CURVE('',#6546,#6546,#721,.T.);
#7936=EDGE_CURVE('',#6547,#6547,#722,.T.);
#7937=EDGE_CURVE('',#6547,#6548,#3750,.T.);
#7938=EDGE_CURVE('',#6548,#6548,#723,.T.);
#7939=EDGE_CURVE('',#6549,#6549,#724,.T.);
#7940=EDGE_CURVE('',#6549,#6550,#3751,.T.);
#7941=EDGE_CURVE('',#6550,#6550,#725,.T.);
#7942=EDGE_CURVE('',#6551,#6552,#3752,.T.);
#7943=EDGE_CURVE('',#6553,#6551,#3753,.T.);
#7944=EDGE_CURVE('',#6553,#6554,#3754,.T.);
#7945=EDGE_CURVE('',#6554,#6552,#3755,.T.);
#7946=EDGE_CURVE('',#6555,#6551,#3756,.T.);
#7947=EDGE_CURVE('',#6556,#6555,#3757,.T.);
#7948=EDGE_CURVE('',#6556,#6553,#3758,.T.);
#7949=EDGE_CURVE('',#6557,#6555,#3759,.T.);
#7950=EDGE_CURVE('',#6558,#6557,#3760,.T.);
#7951=EDGE_CURVE('',#6558,#6556,#3761,.T.);
#7952=EDGE_CURVE('',#6552,#6557,#3762,.T.);
#7953=EDGE_CURVE('',#6554,#6558,#3763,.T.);
#7954=EDGE_CURVE('',#6559,#6559,#726,.T.);
#7955=EDGE_CURVE('',#6559,#6560,#3764,.T.);
#7956=EDGE_CURVE('',#6560,#6560,#727,.T.);
#7957=EDGE_CURVE('',#6561,#6561,#728,.T.);
#7958=EDGE_CURVE('',#6561,#6562,#3765,.T.);
#7959=EDGE_CURVE('',#6562,#6562,#729,.T.);
#7960=EDGE_CURVE('',#6563,#6563,#730,.T.);
#7961=EDGE_CURVE('',#6563,#6564,#3766,.T.);
#7962=EDGE_CURVE('',#6564,#6564,#731,.T.);
#7963=EDGE_CURVE('',#6565,#6565,#732,.T.);
#7964=EDGE_CURVE('',#6565,#6566,#3767,.T.);
#7965=EDGE_CURVE('',#6566,#6566,#733,.T.);
#7966=EDGE_CURVE('',#6567,#6567,#734,.T.);
#7967=EDGE_CURVE('',#6567,#6568,#3768,.T.);
#7968=EDGE_CURVE('',#6568,#6568,#735,.T.);
#7969=EDGE_CURVE('',#6569,#6570,#3769,.T.);
#7970=EDGE_CURVE('',#6571,#6570,#3770,.T.);
#7971=EDGE_CURVE('',#6572,#6571,#3771,.T.);
#7972=EDGE_CURVE('',#6572,#6569,#3772,.T.);
#7973=EDGE_CURVE('',#6573,#6569,#3773,.T.);
#7974=EDGE_CURVE('',#6574,#6572,#3774,.T.);
#7975=EDGE_CURVE('',#6574,#6573,#3775,.T.);
#7976=EDGE_CURVE('',#6575,#6573,#3776,.T.);
#7977=EDGE_CURVE('',#6576,#6574,#3777,.T.);
#7978=EDGE_CURVE('',#6576,#6575,#3778,.T.);
#7979=EDGE_CURVE('',#6570,#6575,#3779,.T.);
#7980=EDGE_CURVE('',#6571,#6576,#3780,.T.);
#7981=EDGE_CURVE('',#6577,#6578,#3781,.T.);
#7982=EDGE_CURVE('',#6579,#6578,#3782,.T.);
#7983=EDGE_CURVE('',#6580,#6579,#3783,.T.);
#7984=EDGE_CURVE('',#6580,#6577,#3784,.T.);
#7985=EDGE_CURVE('',#6578,#6581,#3785,.T.);
#7986=EDGE_CURVE('',#6582,#6581,#3786,.T.);
#7987=EDGE_CURVE('',#6579,#6582,#3787,.T.);
#7988=EDGE_CURVE('',#6581,#6583,#3788,.T.);
#7989=EDGE_CURVE('',#6584,#6583,#3789,.T.);
#7990=EDGE_CURVE('',#6582,#6584,#3790,.T.);
#7991=EDGE_CURVE('',#6583,#6577,#3791,.T.);
#7992=EDGE_CURVE('',#6584,#6580,#3792,.T.);
#7993=EDGE_CURVE('',#6585,#6586,#3793,.T.);
#7994=EDGE_CURVE('',#6587,#6586,#3794,.T.);
#7995=EDGE_CURVE('',#6588,#6587,#3795,.T.);
#7996=EDGE_CURVE('',#6588,#6585,#3796,.T.);
#7997=EDGE_CURVE('',#6586,#6589,#3797,.T.);
#7998=EDGE_CURVE('',#6590,#6589,#3798,.T.);
#7999=EDGE_CURVE('',#6587,#6590,#3799,.T.);
#8000=EDGE_CURVE('',#6589,#6591,#3800,.T.);
#8001=EDGE_CURVE('',#6592,#6591,#3801,.T.);
#8002=EDGE_CURVE('',#6590,#6592,#3802,.T.);
#8003=EDGE_CURVE('',#6591,#6585,#3803,.T.);
#8004=EDGE_CURVE('',#6592,#6588,#3804,.T.);
#8005=EDGE_CURVE('',#6593,#6594,#3805,.T.);
#8006=EDGE_CURVE('',#6595,#6593,#3806,.T.);
#8007=EDGE_CURVE('',#6595,#6596,#3807,.T.);
#8008=EDGE_CURVE('',#6596,#6594,#3808,.T.);
#8009=EDGE_CURVE('',#6594,#6597,#3809,.T.);
#8010=EDGE_CURVE('',#6596,#6598,#3810,.T.);
#8011=EDGE_CURVE('',#6598,#6597,#3811,.T.);
#8012=EDGE_CURVE('',#6597,#6599,#3812,.T.);
#8013=EDGE_CURVE('',#6598,#6600,#3813,.T.);
#8014=EDGE_CURVE('',#6600,#6599,#3814,.T.);
#8015=EDGE_CURVE('',#6599,#6593,#3815,.T.);
#8016=EDGE_CURVE('',#6600,#6595,#3816,.T.);
#8017=EDGE_CURVE('',#6601,#6601,#736,.T.);
#8018=EDGE_CURVE('',#6601,#6602,#3817,.T.);
#8019=EDGE_CURVE('',#6602,#6602,#737,.T.);
#8020=EDGE_CURVE('',#6603,#6603,#738,.T.);
#8021=EDGE_CURVE('',#6603,#6604,#3818,.T.);
#8022=EDGE_CURVE('',#6604,#6604,#739,.T.);
#8023=EDGE_CURVE('',#6605,#6605,#740,.T.);
#8024=EDGE_CURVE('',#6605,#6606,#3819,.T.);
#8025=EDGE_CURVE('',#6606,#6606,#741,.T.);
#8026=EDGE_CURVE('',#6607,#6607,#742,.T.);
#8027=EDGE_CURVE('',#6607,#6608,#3820,.T.);
#8028=EDGE_CURVE('',#6608,#6608,#743,.T.);
#8029=EDGE_CURVE('',#6609,#6609,#744,.T.);
#8030=EDGE_CURVE('',#6609,#6610,#3821,.T.);
#8031=EDGE_CURVE('',#6610,#6610,#745,.T.);
#8032=EDGE_CURVE('',#6611,#6611,#746,.T.);
#8033=EDGE_CURVE('',#6611,#6612,#3822,.T.);
#8034=EDGE_CURVE('',#6612,#6612,#747,.T.);
#8035=EDGE_CURVE('',#6613,#6613,#748,.T.);
#8036=EDGE_CURVE('',#6613,#6614,#3823,.T.);
#8037=EDGE_CURVE('',#6614,#6614,#749,.T.);
#8038=EDGE_CURVE('',#6615,#6615,#750,.T.);
#8039=EDGE_CURVE('',#6615,#6616,#3824,.T.);
#8040=EDGE_CURVE('',#6616,#6616,#751,.T.);
#8041=EDGE_CURVE('',#6617,#6617,#752,.T.);
#8042=EDGE_CURVE('',#6617,#6618,#3825,.T.);
#8043=EDGE_CURVE('',#6618,#6618,#753,.T.);
#8044=EDGE_CURVE('',#6619,#6619,#754,.T.);
#8045=EDGE_CURVE('',#6619,#6620,#3826,.T.);
#8046=EDGE_CURVE('',#6620,#6620,#755,.T.);
#8047=EDGE_CURVE('',#6621,#6621,#756,.T.);
#8048=EDGE_CURVE('',#6621,#6622,#3827,.T.);
#8049=EDGE_CURVE('',#6622,#6622,#757,.T.);
#8050=EDGE_CURVE('',#6623,#6623,#758,.T.);
#8051=EDGE_CURVE('',#6623,#6624,#3828,.T.);
#8052=EDGE_CURVE('',#6624,#6624,#759,.T.);
#8053=EDGE_CURVE('',#6625,#6625,#760,.T.);
#8054=EDGE_CURVE('',#6625,#6626,#3829,.T.);
#8055=EDGE_CURVE('',#6626,#6626,#761,.T.);
#8056=EDGE_CURVE('',#6627,#6627,#762,.T.);
#8057=EDGE_CURVE('',#6627,#6628,#3830,.T.);
#8058=EDGE_CURVE('',#6628,#6628,#763,.T.);
#8059=EDGE_CURVE('',#6629,#6629,#764,.T.);
#8060=EDGE_CURVE('',#6629,#6630,#3831,.T.);
#8061=EDGE_CURVE('',#6630,#6630,#765,.T.);
#8062=EDGE_CURVE('',#6631,#6631,#766,.T.);
#8063=EDGE_CURVE('',#6631,#6632,#3832,.T.);
#8064=EDGE_CURVE('',#6632,#6632,#767,.T.);
#8065=EDGE_CURVE('',#6633,#6633,#768,.T.);
#8066=EDGE_CURVE('',#6633,#6634,#3833,.T.);
#8067=EDGE_CURVE('',#6634,#6634,#769,.T.);
#8068=EDGE_CURVE('',#6635,#6635,#770,.T.);
#8069=EDGE_CURVE('',#6635,#6636,#3834,.T.);
#8070=EDGE_CURVE('',#6636,#6636,#771,.T.);
#8071=EDGE_CURVE('',#6637,#6638,#3835,.T.);
#8072=EDGE_CURVE('',#6639,#6637,#3836,.T.);
#8073=EDGE_CURVE('',#6639,#6640,#3837,.T.);
#8074=EDGE_CURVE('',#6640,#6638,#3838,.T.);
#8075=EDGE_CURVE('',#6641,#6637,#3839,.T.);
#8076=EDGE_CURVE('',#6642,#6641,#3840,.T.);
#8077=EDGE_CURVE('',#6642,#6639,#3841,.T.);
#8078=EDGE_CURVE('',#6643,#6641,#3842,.T.);
#8079=EDGE_CURVE('',#6644,#6643,#3843,.T.);
#8080=EDGE_CURVE('',#6644,#6642,#3844,.T.);
#8081=EDGE_CURVE('',#6638,#6643,#3845,.T.);
#8082=EDGE_CURVE('',#6640,#6644,#3846,.T.);
#8083=EDGE_CURVE('',#6645,#6645,#772,.T.);
#8084=EDGE_CURVE('',#6645,#6646,#3847,.T.);
#8085=EDGE_CURVE('',#6646,#6646,#773,.T.);
#8086=EDGE_CURVE('',#6647,#6647,#774,.T.);
#8087=EDGE_CURVE('',#6647,#6648,#3848,.T.);
#8088=EDGE_CURVE('',#6648,#6648,#775,.T.);
#8089=EDGE_CURVE('',#6649,#6649,#776,.T.);
#8090=EDGE_CURVE('',#6649,#6650,#3849,.T.);
#8091=EDGE_CURVE('',#6650,#6650,#777,.T.);
#8092=EDGE_CURVE('',#6651,#6651,#778,.T.);
#8093=EDGE_CURVE('',#6651,#6652,#3850,.T.);
#8094=EDGE_CURVE('',#6652,#6652,#779,.T.);
#8095=EDGE_CURVE('',#6653,#6653,#780,.T.);
#8096=EDGE_CURVE('',#6653,#6654,#3851,.T.);
#8097=EDGE_CURVE('',#6654,#6654,#781,.T.);
#8098=EDGE_CURVE('',#6655,#6655,#782,.T.);
#8099=EDGE_CURVE('',#6655,#6656,#3852,.T.);
#8100=EDGE_CURVE('',#6656,#6656,#783,.T.);
#8101=EDGE_CURVE('',#6657,#6657,#784,.T.);
#8102=EDGE_CURVE('',#6657,#6658,#3853,.T.);
#8103=EDGE_CURVE('',#6658,#6658,#785,.T.);
#8104=EDGE_CURVE('',#6659,#6659,#786,.T.);
#8105=EDGE_CURVE('',#6659,#6660,#3854,.T.);
#8106=EDGE_CURVE('',#6660,#6660,#787,.T.);
#8107=EDGE_CURVE('',#6661,#6661,#788,.T.);
#8108=EDGE_CURVE('',#6661,#6662,#3855,.T.);
#8109=EDGE_CURVE('',#6662,#6662,#789,.T.);
#8110=EDGE_CURVE('',#6663,#6663,#790,.T.);
#8111=EDGE_CURVE('',#6663,#6664,#3856,.T.);
#8112=EDGE_CURVE('',#6664,#6664,#791,.T.);
#8113=EDGE_CURVE('',#6665,#6665,#792,.T.);
#8114=EDGE_CURVE('',#6665,#6666,#3857,.T.);
#8115=EDGE_CURVE('',#6666,#6666,#793,.T.);
#8116=EDGE_CURVE('',#6667,#6667,#794,.T.);
#8117=EDGE_CURVE('',#6667,#6668,#3858,.T.);
#8118=EDGE_CURVE('',#6668,#6668,#795,.T.);
#8119=EDGE_CURVE('',#6669,#6669,#796,.T.);
#8120=EDGE_CURVE('',#6669,#6670,#3859,.T.);
#8121=EDGE_CURVE('',#6670,#6670,#797,.T.);
#8122=EDGE_CURVE('',#6671,#6671,#798,.T.);
#8123=EDGE_CURVE('',#6671,#6672,#3860,.T.);
#8124=EDGE_CURVE('',#6672,#6672,#799,.T.);
#8125=EDGE_CURVE('',#6673,#6673,#800,.T.);
#8126=EDGE_CURVE('',#6673,#6674,#3861,.T.);
#8127=EDGE_CURVE('',#6674,#6674,#801,.T.);
#8128=EDGE_CURVE('',#6675,#6675,#802,.T.);
#8129=EDGE_CURVE('',#6675,#6676,#3862,.T.);
#8130=EDGE_CURVE('',#6676,#6676,#803,.T.);
#8131=EDGE_CURVE('',#6677,#6677,#804,.T.);
#8132=EDGE_CURVE('',#6677,#6678,#3863,.T.);
#8133=EDGE_CURVE('',#6678,#6678,#805,.T.);
#8134=EDGE_CURVE('',#6679,#6679,#806,.T.);
#8135=EDGE_CURVE('',#6679,#6680,#3864,.T.);
#8136=EDGE_CURVE('',#6680,#6680,#807,.T.);
#8137=EDGE_CURVE('',#6681,#6681,#808,.T.);
#8138=EDGE_CURVE('',#6681,#6682,#3865,.T.);
#8139=EDGE_CURVE('',#6682,#6682,#809,.T.);
#8140=EDGE_CURVE('',#6683,#6683,#810,.T.);
#8141=EDGE_CURVE('',#6683,#6684,#3866,.T.);
#8142=EDGE_CURVE('',#6684,#6684,#811,.T.);
#8143=EDGE_CURVE('',#6685,#6685,#812,.T.);
#8144=EDGE_CURVE('',#6685,#6686,#3867,.T.);
#8145=EDGE_CURVE('',#6686,#6686,#813,.T.);
#8146=EDGE_CURVE('',#6687,#6687,#814,.T.);
#8147=EDGE_CURVE('',#6687,#6688,#3868,.T.);
#8148=EDGE_CURVE('',#6688,#6688,#815,.T.);
#8149=EDGE_CURVE('',#6689,#6689,#816,.T.);
#8150=EDGE_CURVE('',#6689,#6690,#3869,.T.);
#8151=EDGE_CURVE('',#6690,#6690,#817,.T.);
#8152=EDGE_CURVE('',#6691,#6691,#818,.T.);
#8153=EDGE_CURVE('',#6691,#6692,#3870,.T.);
#8154=EDGE_CURVE('',#6692,#6692,#819,.T.);
#8155=EDGE_CURVE('',#6693,#6694,#3871,.T.);
#8156=EDGE_CURVE('',#6695,#6693,#3872,.T.);
#8157=EDGE_CURVE('',#6696,#6695,#3873,.T.);
#8158=EDGE_CURVE('',#6697,#6696,#3874,.T.);
#8159=EDGE_CURVE('',#6698,#6697,#644,.T.);
#8160=EDGE_CURVE('',#6699,#6698,#3875,.T.);
#8161=EDGE_CURVE('',#6700,#6699,#645,.T.);
#8162=EDGE_CURVE('',#6701,#6700,#3876,.T.);
#8163=EDGE_CURVE('',#6694,#6701,#646,.T.);
#8164=EDGE_CURVE('',#6702,#6703,#3877,.T.);
#8165=EDGE_CURVE('',#6704,#6702,#3878,.T.);
#8166=EDGE_CURVE('',#6705,#6704,#647,.T.);
#8167=EDGE_CURVE('',#6706,#6705,#3879,.T.);
#8168=EDGE_CURVE('',#6707,#6706,#648,.T.);
#8169=EDGE_CURVE('',#6708,#6707,#3880,.T.);
#8170=EDGE_CURVE('',#6709,#6708,#649,.T.);
#8171=EDGE_CURVE('',#6710,#6709,#3881,.T.);
#8172=EDGE_CURVE('',#6703,#6710,#3882,.T.);
#8173=EDGE_CURVE('',#6695,#6703,#3883,.T.);
#8174=EDGE_CURVE('',#6693,#6702,#3884,.T.);
#8175=EDGE_CURVE('',#6696,#6710,#3885,.T.);
#8176=EDGE_CURVE('',#6697,#6709,#3886,.T.);
#8177=EDGE_CURVE('',#6698,#6708,#3887,.T.);
#8178=EDGE_CURVE('',#6699,#6707,#3888,.T.);
#8179=EDGE_CURVE('',#6700,#6706,#3889,.T.);
#8180=EDGE_CURVE('',#6701,#6705,#3890,.T.);
#8181=EDGE_CURVE('',#6694,#6704,#3891,.T.);
#8182=EDGE_CURVE('',#6711,#6712,#3892,.T.);
#8183=EDGE_CURVE('',#6713,#6711,#650,.T.);
#8184=EDGE_CURVE('',#6714,#6713,#3893,.T.);
#8185=EDGE_CURVE('',#6715,#6714,#651,.T.);
#8186=EDGE_CURVE('',#6716,#6715,#3894,.T.);
#8187=EDGE_CURVE('',#6717,#6716,#652,.T.);
#8188=EDGE_CURVE('',#6718,#6717,#3895,.T.);
#8189=EDGE_CURVE('',#6719,#6718,#3896,.T.);
#8190=EDGE_CURVE('',#6712,#6719,#3897,.T.);
#8191=EDGE_CURVE('',#6720,#6721,#3898,.T.);
#8192=EDGE_CURVE('',#6722,#6720,#3899,.T.);
#8193=EDGE_CURVE('',#6723,#6722,#3900,.T.);
#8194=EDGE_CURVE('',#6724,#6723,#653,.T.);
#8195=EDGE_CURVE('',#6725,#6724,#3901,.T.);
#8196=EDGE_CURVE('',#6726,#6725,#654,.T.);
#8197=EDGE_CURVE('',#6727,#6726,#3902,.T.);
#8198=EDGE_CURVE('',#6728,#6727,#655,.T.);
#8199=EDGE_CURVE('',#6721,#6728,#3903,.T.);
#8200=EDGE_CURVE('',#6721,#6712,#3904,.T.);
#8201=EDGE_CURVE('',#6720,#6719,#3905,.T.);
#8202=EDGE_CURVE('',#6722,#6718,#3906,.T.);
#8203=EDGE_CURVE('',#6723,#6717,#3907,.T.);
#8204=EDGE_CURVE('',#6724,#6716,#3908,.T.);
#8205=EDGE_CURVE('',#6725,#6715,#3909,.T.);
#8206=EDGE_CURVE('',#6726,#6714,#3910,.T.);
#8207=EDGE_CURVE('',#6727,#6713,#3911,.T.);
#8208=EDGE_CURVE('',#6728,#6711,#3912,.T.);
#8209=EDGE_CURVE('',#6729,#6730,#3913,.T.);
#8210=EDGE_CURVE('',#6731,#6729,#656,.T.);
#8211=EDGE_CURVE('',#6732,#6731,#3914,.T.);
#8212=EDGE_CURVE('',#6733,#6732,#657,.T.);
#8213=EDGE_CURVE('',#6734,#6733,#3915,.T.);
#8214=EDGE_CURVE('',#6735,#6734,#658,.T.);
#8215=EDGE_CURVE('',#6736,#6735,#3916,.T.);
#8216=EDGE_CURVE('',#6737,#6736,#3917,.T.);
#8217=EDGE_CURVE('',#6730,#6737,#3918,.T.);
#8218=EDGE_CURVE('',#6738,#6739,#3919,.T.);
#8219=EDGE_CURVE('',#6740,#6738,#3920,.T.);
#8220=EDGE_CURVE('',#6741,#6740,#3921,.T.);
#8221=EDGE_CURVE('',#6742,#6741,#659,.T.);
#8222=EDGE_CURVE('',#6743,#6742,#3922,.T.);
#8223=EDGE_CURVE('',#6744,#6743,#660,.T.);
#8224=EDGE_CURVE('',#6745,#6744,#3923,.T.);
#8225=EDGE_CURVE('',#6746,#6745,#661,.T.);
#8226=EDGE_CURVE('',#6739,#6746,#3924,.T.);
#8227=EDGE_CURVE('',#6739,#6730,#3925,.T.);
#8228=EDGE_CURVE('',#6738,#6737,#3926,.T.);
#8229=EDGE_CURVE('',#6740,#6736,#3927,.T.);
#8230=EDGE_CURVE('',#6741,#6735,#3928,.T.);
#8231=EDGE_CURVE('',#6742,#6734,#3929,.T.);
#8232=EDGE_CURVE('',#6743,#6733,#3930,.T.);
#8233=EDGE_CURVE('',#6744,#6732,#3931,.T.);
#8234=EDGE_CURVE('',#6745,#6731,#3932,.T.);
#8235=EDGE_CURVE('',#6746,#6729,#3933,.T.);
#8236=EDGE_CURVE('',#6747,#6747,#820,.T.);
#8237=EDGE_CURVE('',#6747,#6748,#3934,.T.);
#8238=EDGE_CURVE('',#6748,#6748,#821,.T.);
#8239=EDGE_CURVE('',#6749,#6750,#822,.T.);
#8240=EDGE_CURVE('',#6750,#6751,#3935,.T.);
#8241=EDGE_CURVE('',#6752,#6751,#823,.T.);
#8242=EDGE_CURVE('',#6749,#6752,#3936,.T.);
#8243=EDGE_CURVE('',#6753,#6752,#824,.T.);
#8244=EDGE_CURVE('',#6754,#6753,#3937,.T.);
#8245=EDGE_CURVE('',#6754,#6749,#825,.T.);
#8246=EDGE_CURVE('',#6755,#6753,#3938,.T.);
#8247=EDGE_CURVE('',#6756,#6755,#3939,.T.);
#8248=EDGE_CURVE('',#6756,#6754,#3940,.T.);
#8249=EDGE_CURVE('',#6757,#6755,#3941,.T.);
#8250=EDGE_CURVE('',#6758,#6757,#3942,.T.);
#8251=EDGE_CURVE('',#6758,#6756,#3943,.T.);
#8252=EDGE_CURVE('',#6759,#6757,#3944,.T.);
#8253=EDGE_CURVE('',#6760,#6759,#3945,.T.);
#8254=EDGE_CURVE('',#6760,#6758,#3946,.T.);
#8255=EDGE_CURVE('',#6751,#6759,#3947,.T.);
#8256=EDGE_CURVE('',#6750,#6760,#3948,.T.);
#8257=EDGE_CURVE('',#6761,#6761,#826,.T.);
#8258=EDGE_CURVE('',#6761,#6762,#3949,.T.);
#8259=EDGE_CURVE('',#6762,#6762,#827,.T.);
#8260=EDGE_CURVE('',#6763,#6764,#3950,.T.);
#8261=EDGE_CURVE('',#6764,#6765,#3951,.T.);
#8262=EDGE_CURVE('',#6765,#6766,#3952,.T.);
#8263=EDGE_CURVE('',#6766,#6767,#828,.T.);
#8264=EDGE_CURVE('',#6767,#6768,#3953,.T.);
#8265=EDGE_CURVE('',#6768,#6763,#3954,.T.);
#8266=EDGE_CURVE('',#6769,#6770,#3955,.T.);
#8267=EDGE_CURVE('',#6771,#6769,#3956,.T.);
#8268=EDGE_CURVE('',#6772,#6771,#3957,.T.);
#8269=EDGE_CURVE('',#6773,#6772,#829,.T.);
#8270=EDGE_CURVE('',#6774,#6773,#3958,.T.);
#8271=EDGE_CURVE('',#6770,#6774,#3959,.T.);
#8272=EDGE_CURVE('',#6764,#6770,#3960,.T.);
#8273=EDGE_CURVE('',#6763,#6769,#3961,.T.);
#8274=EDGE_CURVE('',#6765,#6774,#3962,.T.);
#8275=EDGE_CURVE('',#6766,#6773,#3963,.T.);
#8276=EDGE_CURVE('',#6767,#6772,#3964,.T.);
#8277=EDGE_CURVE('',#6768,#6771,#3965,.T.);
#8278=EDGE_CURVE('',#6775,#6775,#830,.T.);
#8279=EDGE_CURVE('',#6775,#6776,#3966,.T.);
#8280=EDGE_CURVE('',#6776,#6776,#831,.T.);
#8281=EDGE_CURVE('',#6777,#6778,#832,.T.);
#8282=EDGE_CURVE('',#6777,#6779,#3967,.T.);
#8283=EDGE_CURVE('',#6779,#6780,#833,.T.);
#8284=EDGE_CURVE('',#6778,#6780,#3968,.T.);
#8285=EDGE_CURVE('',#6781,#6779,#834,.T.);
#8286=EDGE_CURVE('',#6782,#6777,#835,.T.);
#8287=EDGE_CURVE('',#6782,#6781,#3969,.T.);
#8288=EDGE_CURVE('',#6783,#6781,#3970,.T.);
#8289=EDGE_CURVE('',#6784,#6782,#3971,.T.);
#8290=EDGE_CURVE('',#6784,#6783,#3972,.T.);
#8291=EDGE_CURVE('',#6785,#6783,#3973,.T.);
#8292=EDGE_CURVE('',#6786,#6784,#3974,.T.);
#8293=EDGE_CURVE('',#6786,#6785,#3975,.T.);
#8294=EDGE_CURVE('',#6787,#6785,#3976,.T.);
#8295=EDGE_CURVE('',#6788,#6786,#3977,.T.);
#8296=EDGE_CURVE('',#6788,#6787,#3978,.T.);
#8297=EDGE_CURVE('',#6780,#6787,#3979,.T.);
#8298=EDGE_CURVE('',#6778,#6788,#3980,.T.);
#8299=EDGE_CURVE('',#6789,#6789,#836,.T.);
#8300=EDGE_CURVE('',#6789,#6790,#3981,.T.);
#8301=EDGE_CURVE('',#6790,#6790,#837,.T.);
#8302=EDGE_CURVE('',#6791,#6792,#3982,.T.);
#8303=EDGE_CURVE('',#6793,#6791,#3983,.T.);
#8304=EDGE_CURVE('',#6794,#6793,#3984,.T.);
#8305=EDGE_CURVE('',#6795,#6794,#838,.T.);
#8306=EDGE_CURVE('',#6796,#6795,#3985,.T.);
#8307=EDGE_CURVE('',#6792,#6796,#3986,.T.);
#8308=EDGE_CURVE('',#6797,#6798,#3987,.T.);
#8309=EDGE_CURVE('',#6798,#6799,#3988,.T.);
#8310=EDGE_CURVE('',#6799,#6800,#3989,.T.);
#8311=EDGE_CURVE('',#6800,#6801,#839,.T.);
#8312=EDGE_CURVE('',#6801,#6802,#3990,.T.);
#8313=EDGE_CURVE('',#6802,#6797,#3991,.T.);
#8314=EDGE_CURVE('',#6791,#6797,#3992,.T.);
#8315=EDGE_CURVE('',#6792,#6798,#3993,.T.);
#8316=EDGE_CURVE('',#6796,#6799,#3994,.T.);
#8317=EDGE_CURVE('',#6795,#6800,#3995,.T.);
#8318=EDGE_CURVE('',#6794,#6801,#3996,.T.);
#8319=EDGE_CURVE('',#6793,#6802,#3997,.T.);
#8320=EDGE_CURVE('',#6803,#6804,#840,.T.);
#8321=EDGE_CURVE('',#6804,#6805,#3998,.T.);
#8322=EDGE_CURVE('',#6805,#6806,#841,.T.);
#8323=EDGE_CURVE('',#6803,#6806,#3999,.T.);
#8324=EDGE_CURVE('',#6807,#6808,#842,.T.);
#8325=EDGE_CURVE('',#6808,#6809,#4000,.T.);
#8326=EDGE_CURVE('',#6809,#6810,#843,.T.);
#8327=EDGE_CURVE('',#6807,#6810,#4001,.T.);
#8328=EDGE_CURVE('',#6811,#6812,#844,.T.);
#8329=EDGE_CURVE('',#6813,#6811,#4002,.T.);
#8330=EDGE_CURVE('',#6814,#6813,#845,.T.);
#8331=EDGE_CURVE('',#6814,#6812,#4003,.T.);
#8332=EDGE_CURVE('',#6815,#6816,#846,.T.);
#8333=EDGE_CURVE('',#6817,#6815,#4004,.T.);
#8334=EDGE_CURVE('',#6817,#6818,#662,.T.);
#8335=EDGE_CURVE('',#6818,#6816,#4005,.T.);
#8336=EDGE_CURVE('',#6819,#6811,#4006,.T.);
#8337=EDGE_CURVE('',#6820,#6819,#4007,.T.);
#8338=EDGE_CURVE('',#6813,#6820,#4008,.T.);
#8339=EDGE_CURVE('',#6821,#6815,#4009,.T.);
#8340=EDGE_CURVE('',#6822,#6821,#4010,.T.);
#8341=EDGE_CURVE('',#6822,#6817,#4011,.T.);
#8342=EDGE_CURVE('',#6823,#6824,#4012,.T.);
#8343=EDGE_CURVE('',#6825,#6823,#663,.T.);
#8344=EDGE_CURVE('',#6826,#6825,#4013,.T.);
#8345=EDGE_CURVE('',#6827,#6826,#664,.T.);
#8346=EDGE_CURVE('',#6828,#6827,#4014,.T.);
#8347=EDGE_CURVE('',#6829,#6828,#665,.T.);
#8348=EDGE_CURVE('',#6830,#6829,#4015,.T.);
#8349=EDGE_CURVE('',#6831,#6830,#4016,.T.);
#8350=EDGE_CURVE('',#6824,#6831,#4017,.T.);
#8351=EDGE_CURVE('',#6832,#6822,#4018,.T.);
#8352=EDGE_CURVE('',#6833,#6832,#4019,.T.);
#8353=EDGE_CURVE('',#6834,#6833,#4020,.T.);
#8354=EDGE_CURVE('',#6835,#6834,#666,.T.);
#8355=EDGE_CURVE('',#6836,#6835,#4021,.T.);
#8356=EDGE_CURVE('',#6837,#6836,#667,.T.);
#8357=EDGE_CURVE('',#6818,#6837,#4022,.T.);
#8358=EDGE_CURVE('',#6806,#6819,#4023,.T.);
#8359=EDGE_CURVE('',#6838,#6805,#4024,.T.);
#8360=EDGE_CURVE('',#6838,#6824,#4025,.T.);
#8361=EDGE_CURVE('',#6832,#6831,#4026,.T.);
#8362=EDGE_CURVE('',#6810,#6821,#4027,.T.);
#8363=EDGE_CURVE('',#6820,#6809,#4028,.T.);
#8364=EDGE_CURVE('',#6833,#6830,#4029,.T.);
#8365=EDGE_CURVE('',#6834,#6829,#4030,.T.);
#8366=EDGE_CURVE('',#6835,#6828,#4031,.T.);
#8367=EDGE_CURVE('',#6836,#6827,#4032,.T.);
#8368=EDGE_CURVE('',#6837,#6826,#4033,.T.);
#8369=EDGE_CURVE('',#6812,#6803,#4034,.T.);
#8370=EDGE_CURVE('',#6808,#6814,#4035,.T.);
#8371=EDGE_CURVE('',#6816,#6807,#4036,.T.);
#8372=EDGE_CURVE('',#6839,#6825,#4037,.T.);
#8373=EDGE_CURVE('',#6804,#6839,#4038,.T.);
#8374=EDGE_CURVE('',#6839,#6840,#847,.T.);
#8375=EDGE_CURVE('',#6840,#6823,#4039,.T.);
#8376=EDGE_CURVE('',#6840,#6838,#4040,.T.);
#8377=EDGE_CURVE('',#6841,#6841,#848,.T.);
#8378=EDGE_CURVE('',#6841,#6842,#4041,.T.);
#8379=EDGE_CURVE('',#6842,#6842,#849,.T.);
#8380=EDGE_CURVE('',#6843,#6844,#4042,.T.);
#8381=EDGE_CURVE('',#6845,#6843,#4043,.T.);
#8382=EDGE_CURVE('',#6846,#6845,#4044,.T.);
#8383=EDGE_CURVE('',#6847,#6846,#850,.T.);
#8384=EDGE_CURVE('',#6848,#6847,#4045,.T.);
#8385=EDGE_CURVE('',#6844,#6848,#4046,.T.);
#8386=EDGE_CURVE('',#6849,#6850,#4047,.T.);
#8387=EDGE_CURVE('',#6850,#6851,#4048,.T.);
#8388=EDGE_CURVE('',#6851,#6852,#4049,.T.);
#8389=EDGE_CURVE('',#6852,#6853,#851,.T.);
#8390=EDGE_CURVE('',#6853,#6854,#4050,.T.);
#8391=EDGE_CURVE('',#6854,#6849,#4051,.T.);
#8392=EDGE_CURVE('',#6843,#6849,#4052,.T.);
#8393=EDGE_CURVE('',#6844,#6850,#4053,.T.);
#8394=EDGE_CURVE('',#6848,#6851,#4054,.T.);
#8395=EDGE_CURVE('',#6847,#6852,#4055,.T.);
#8396=EDGE_CURVE('',#6846,#6853,#4056,.T.);
#8397=EDGE_CURVE('',#6845,#6854,#4057,.T.);
#8398=EDGE_CURVE('',#6855,#6855,#852,.T.);
#8399=EDGE_CURVE('',#6855,#6856,#4058,.T.);
#8400=EDGE_CURVE('',#6856,#6856,#853,.T.);
#8401=EDGE_CURVE('',#6857,#6858,#4059,.T.);
#8402=EDGE_CURVE('',#6858,#6859,#4060,.T.);
#8403=EDGE_CURVE('',#6859,#6860,#4061,.T.);
#8404=EDGE_CURVE('',#6860,#6861,#854,.T.);
#8405=EDGE_CURVE('',#6861,#6862,#4062,.T.);
#8406=EDGE_CURVE('',#6862,#6857,#4063,.T.);
#8407=EDGE_CURVE('',#6863,#6864,#4064,.T.);
#8408=EDGE_CURVE('',#6865,#6863,#4065,.T.);
#8409=EDGE_CURVE('',#6866,#6865,#4066,.T.);
#8410=EDGE_CURVE('',#6867,#6866,#855,.T.);
#8411=EDGE_CURVE('',#6868,#6867,#4067,.T.);
#8412=EDGE_CURVE('',#6864,#6868,#4068,.T.);
#8413=EDGE_CURVE('',#6858,#6864,#4069,.T.);
#8414=EDGE_CURVE('',#6857,#6863,#4070,.T.);
#8415=EDGE_CURVE('',#6859,#6868,#4071,.T.);
#8416=EDGE_CURVE('',#6860,#6867,#4072,.T.);
#8417=EDGE_CURVE('',#6861,#6866,#4073,.T.);
#8418=EDGE_CURVE('',#6862,#6865,#4074,.T.);
#8419=EDGE_CURVE('',#6869,#6870,#4075,.T.);
#8420=EDGE_CURVE('',#6871,#6869,#4076,.T.);
#8421=EDGE_CURVE('',#6871,#6872,#4077,.T.);
#8422=EDGE_CURVE('',#6872,#6870,#4078,.T.);
#8423=EDGE_CURVE('',#6873,#6869,#4079,.T.);
#8424=EDGE_CURVE('',#6874,#6873,#4080,.T.);
#8425=EDGE_CURVE('',#6874,#6871,#4081,.T.);
#8426=EDGE_CURVE('',#6875,#6873,#856,.T.);
#8427=EDGE_CURVE('',#6876,#6875,#4082,.T.);
#8428=EDGE_CURVE('',#6876,#6874,#857,.T.);
#8429=EDGE_CURVE('',#6877,#6875,#4083,.T.);
#8430=EDGE_CURVE('',#6878,#6877,#4084,.T.);
#8431=EDGE_CURVE('',#6878,#6876,#4085,.T.);
#8432=EDGE_CURVE('',#6879,#6877,#4086,.T.);
#8433=EDGE_CURVE('',#6880,#6879,#4087,.T.);
#8434=EDGE_CURVE('',#6880,#6878,#4088,.T.);
#8435=EDGE_CURVE('',#6881,#6879,#4089,.T.);
#8436=EDGE_CURVE('',#6882,#6881,#4090,.T.);
#8437=EDGE_CURVE('',#6882,#6880,#4091,.T.);
#8438=EDGE_CURVE('',#6883,#6881,#858,.T.);
#8439=EDGE_CURVE('',#6884,#6883,#4092,.T.);
#8440=EDGE_CURVE('',#6884,#6882,#859,.T.);
#8441=EDGE_CURVE('',#6885,#6883,#4093,.T.);
#8442=EDGE_CURVE('',#6886,#6885,#4094,.T.);
#8443=EDGE_CURVE('',#6886,#6884,#4095,.T.);
#8444=EDGE_CURVE('',#6887,#6885,#4096,.T.);
#8445=EDGE_CURVE('',#6888,#6887,#4097,.T.);
#8446=EDGE_CURVE('',#6888,#6886,#4098,.T.);
#8447=EDGE_CURVE('',#6889,#6887,#4099,.T.);
#8448=EDGE_CURVE('',#6890,#6889,#4100,.T.);
#8449=EDGE_CURVE('',#6890,#6888,#4101,.T.);
#8450=EDGE_CURVE('',#6891,#6889,#4102,.T.);
#8451=EDGE_CURVE('',#6892,#6891,#4103,.T.);
#8452=EDGE_CURVE('',#6892,#6890,#4104,.T.);
#8453=EDGE_CURVE('',#6870,#6891,#4105,.T.);
#8454=EDGE_CURVE('',#6872,#6892,#4106,.T.);
#8455=EDGE_CURVE('',#6893,#6893,#860,.T.);
#8456=EDGE_CURVE('',#6893,#6894,#4107,.T.);
#8457=EDGE_CURVE('',#6894,#6894,#861,.T.);
#8458=EDGE_CURVE('',#6895,#6896,#862,.T.);
#8459=EDGE_CURVE('',#6895,#6897,#4108,.T.);
#8460=EDGE_CURVE('',#6897,#6898,#863,.T.);
#8461=EDGE_CURVE('',#6896,#6898,#4109,.T.);
#8462=EDGE_CURVE('',#6899,#6895,#864,.T.);
#8463=EDGE_CURVE('',#6899,#6900,#4110,.T.);
#8464=EDGE_CURVE('',#6900,#6897,#865,.T.);
#8465=EDGE_CURVE('',#6896,#6901,#4111,.T.);
#8466=EDGE_CURVE('',#6901,#6902,#4112,.T.);
#8467=EDGE_CURVE('',#6902,#6903,#4113,.T.);
#8468=EDGE_CURVE('',#6903,#6899,#4114,.T.);
#8469=EDGE_CURVE('',#6904,#6900,#4115,.T.);
#8470=EDGE_CURVE('',#6905,#6904,#4116,.T.);
#8471=EDGE_CURVE('',#6906,#6905,#4117,.T.);
#8472=EDGE_CURVE('',#6898,#6906,#4118,.T.);
#8473=EDGE_CURVE('',#6901,#6906,#4119,.T.);
#8474=EDGE_CURVE('',#6902,#6905,#4120,.T.);
#8475=EDGE_CURVE('',#6903,#6904,#4121,.T.);
#8476=EDGE_CURVE('',#6907,#6907,#866,.T.);
#8477=EDGE_CURVE('',#6907,#6908,#4122,.T.);
#8478=EDGE_CURVE('',#6908,#6908,#867,.T.);
#8479=EDGE_CURVE('',#6909,#6910,#868,.T.);
#8480=EDGE_CURVE('',#6910,#6911,#4123,.T.);
#8481=EDGE_CURVE('',#6912,#6911,#869,.T.);
#8482=EDGE_CURVE('',#6909,#6912,#4124,.T.);
#8483=EDGE_CURVE('',#6913,#6909,#870,.T.);
#8484=EDGE_CURVE('',#6914,#6912,#871,.T.);
#8485=EDGE_CURVE('',#6913,#6914,#4125,.T.);
#8486=EDGE_CURVE('',#6915,#6913,#4126,.T.);
#8487=EDGE_CURVE('',#6916,#6915,#4127,.T.);
#8488=EDGE_CURVE('',#6917,#6916,#4128,.T.);
#8489=EDGE_CURVE('',#6910,#6917,#4129,.T.);
#8490=EDGE_CURVE('',#6911,#6918,#4130,.T.);
#8491=EDGE_CURVE('',#6918,#6919,#4131,.T.);
#8492=EDGE_CURVE('',#6919,#6920,#4132,.T.);
#8493=EDGE_CURVE('',#6920,#6914,#4133,.T.);
#8494=EDGE_CURVE('',#6917,#6918,#4134,.T.);
#8495=EDGE_CURVE('',#6916,#6919,#4135,.T.);
#8496=EDGE_CURVE('',#6915,#6920,#4136,.T.);
#8497=EDGE_CURVE('',#6921,#6922,#872,.T.);
#8498=EDGE_CURVE('',#6922,#6923,#873,.T.);
#8499=EDGE_CURVE('',#6923,#6923,#874,.T.);
#8500=EDGE_CURVE('',#6922,#6921,#875,.T.);
#8501=EDGE_CURVE('',#6924,#6924,#876,.T.);
#8502=EDGE_CURVE('',#6924,#6925,#877,.T.);
#8503=EDGE_CURVE('',#6926,#6925,#878,.T.);
#8504=EDGE_CURVE('',#6925,#6926,#879,.T.);
#8505=EDGE_CURVE('',#6923,#6927,#4137,.T.);
#8506=EDGE_CURVE('',#6927,#6927,#880,.T.);
#8507=EDGE_CURVE('',#6926,#6921,#4138,.T.);
#8508=EDGE_CURVE('',#6928,#6928,#881,.T.);
#8509=EDGE_CURVE('',#6928,#6924,#4139,.T.);
#8510=EDGE_CURVE('',#6929,#6929,#882,.T.);
#8511=EDGE_CURVE('',#6929,#6930,#4140,.T.);
#8512=EDGE_CURVE('',#6930,#6930,#883,.T.);
#8513=EDGE_CURVE('',#6931,#6931,#884,.T.);
#8514=EDGE_CURVE('',#6931,#6929,#4141,.T.);
#8515=EDGE_CURVE('',#6932,#6933,#408,.T.);
#8516=EDGE_CURVE('',#6934,#6932,#4142,.T.);
#8517=EDGE_CURVE('',#6935,#6934,#4143,.T.);
#8518=EDGE_CURVE('',#6935,#6936,#4144,.T.);
#8519=EDGE_CURVE('',#6933,#6936,#409,.T.);
#8520=EDGE_CURVE('',#6937,#6938,#410,.T.);
#8521=EDGE_CURVE('',#6939,#6937,#4145,.T.);
#8522=EDGE_CURVE('',#6934,#6939,#4146,.T.);
#8523=EDGE_CURVE('',#6938,#6932,#411,.T.);
#8524=EDGE_CURVE('',#6940,#6941,#412,.T.);
#8525=EDGE_CURVE('',#6942,#6940,#4147,.T.);
#8526=EDGE_CURVE('',#6939,#6942,#4148,.T.);
#8527=EDGE_CURVE('',#6941,#6937,#413,.T.);
#8528=EDGE_CURVE('',#6943,#6944,#414,.T.);
#8529=EDGE_CURVE('',#6945,#6943,#4149,.T.);
#8530=EDGE_CURVE('',#6942,#6945,#4150,.T.);
#8531=EDGE_CURVE('',#6944,#6940,#415,.T.);
#8532=EDGE_CURVE('',#6946,#6947,#416,.T.);
#8533=EDGE_CURVE('',#6948,#6946,#4151,.T.);
#8534=EDGE_CURVE('',#6945,#6948,#4152,.T.);
#8535=EDGE_CURVE('',#6947,#6943,#417,.T.);
#8536=EDGE_CURVE('',#6936,#6949,#418,.T.);
#8537=EDGE_CURVE('',#6948,#6935,#4153,.T.);
#8538=EDGE_CURVE('',#6949,#6946,#419,.T.);
#8539=EDGE_CURVE('',#6947,#6949,#885,.T.);
#8540=EDGE_CURVE('',#6944,#6947,#886,.T.);
#8541=EDGE_CURVE('',#6941,#6944,#887,.T.);
#8542=EDGE_CURVE('',#6941,#6938,#888,.T.);
#8543=EDGE_CURVE('',#6933,#6938,#889,.T.);
#8544=EDGE_CURVE('',#6949,#6933,#890,.T.);
#8545=EDGE_CURVE('',#6950,#6950,#891,.T.);
#8546=EDGE_CURVE('',#6950,#6951,#4154,.T.);
#8547=EDGE_CURVE('',#6951,#6951,#892,.T.);
#8548=EDGE_CURVE('',#6952,#6952,#893,.T.);
#8549=EDGE_CURVE('',#6952,#6950,#4155,.T.);
#8550=EDGE_CURVE('',#6953,#6954,#420,.T.);
#8551=EDGE_CURVE('',#6955,#6953,#4156,.T.);
#8552=EDGE_CURVE('',#6956,#6955,#4157,.T.);
#8553=EDGE_CURVE('',#6956,#6957,#4158,.T.);
#8554=EDGE_CURVE('',#6954,#6957,#421,.T.);
#8555=EDGE_CURVE('',#6958,#6959,#422,.T.);
#8556=EDGE_CURVE('',#6960,#6958,#4159,.T.);
#8557=EDGE_CURVE('',#6955,#6960,#4160,.T.);
#8558=EDGE_CURVE('',#6959,#6953,#423,.T.);
#8559=EDGE_CURVE('',#6961,#6962,#424,.T.);
#8560=EDGE_CURVE('',#6963,#6961,#4161,.T.);
#8561=EDGE_CURVE('',#6960,#6963,#4162,.T.);
#8562=EDGE_CURVE('',#6962,#6958,#425,.T.);
#8563=EDGE_CURVE('',#6964,#6965,#426,.T.);
#8564=EDGE_CURVE('',#6966,#6964,#4163,.T.);
#8565=EDGE_CURVE('',#6963,#6966,#4164,.T.);
#8566=EDGE_CURVE('',#6965,#6961,#427,.T.);
#8567=EDGE_CURVE('',#6967,#6968,#428,.T.);
#8568=EDGE_CURVE('',#6969,#6967,#4165,.T.);
#8569=EDGE_CURVE('',#6966,#6969,#4166,.T.);
#8570=EDGE_CURVE('',#6968,#6964,#429,.T.);
#8571=EDGE_CURVE('',#6957,#6970,#430,.T.);
#8572=EDGE_CURVE('',#6969,#6956,#4167,.T.);
#8573=EDGE_CURVE('',#6970,#6967,#431,.T.);
#8574=EDGE_CURVE('',#6968,#6970,#894,.T.);
#8575=EDGE_CURVE('',#6965,#6968,#895,.T.);
#8576=EDGE_CURVE('',#6962,#6965,#896,.T.);
#8577=EDGE_CURVE('',#6962,#6959,#897,.T.);
#8578=EDGE_CURVE('',#6954,#6959,#898,.T.);
#8579=EDGE_CURVE('',#6970,#6954,#899,.T.);
#8580=EDGE_CURVE('',#6971,#6971,#900,.T.);
#8581=EDGE_CURVE('',#6971,#6972,#4168,.T.);
#8582=EDGE_CURVE('',#6972,#6973,#901,.T.);
#8583=EDGE_CURVE('',#6973,#6972,#902,.T.);
#8584=EDGE_CURVE('',#6974,#6975,#903,.T.);
#8585=EDGE_CURVE('',#6975,#6973,#4169,.T.);
#8586=EDGE_CURVE('',#6975,#6974,#904,.T.);
#8587=EDGE_CURVE('',#6976,#6976,#905,.T.);
#8588=EDGE_CURVE('',#6976,#6977,#4170,.T.);
#8589=EDGE_CURVE('',#6977,#6977,#906,.T.);
#8590=EDGE_CURVE('',#6974,#6976,#4171,.T.);
#8591=EDGE_CURVE('',#6978,#6979,#4172,.T.);
#8592=EDGE_CURVE('',#6979,#6980,#432,.T.);
#8593=EDGE_CURVE('',#6980,#6981,#433,.T.);
#8594=EDGE_CURVE('',#6982,#6981,#4173,.T.);
#8595=EDGE_CURVE('',#6983,#6982,#434,.T.);
#8596=EDGE_CURVE('',#6978,#6983,#435,.T.);
#8597=EDGE_CURVE('',#6981,#6984,#436,.T.);
#8598=EDGE_CURVE('',#6984,#6985,#437,.T.);
#8599=EDGE_CURVE('',#6986,#6985,#4174,.T.);
#8600=EDGE_CURVE('',#6987,#6986,#438,.T.);
#8601=EDGE_CURVE('',#6982,#6987,#439,.T.);
#8602=EDGE_CURVE('',#6988,#6989,#440,.T.);
#8603=EDGE_CURVE('',#6990,#6988,#4175,.T.);
#8604=EDGE_CURVE('',#6990,#6991,#441,.T.);
#8605=EDGE_CURVE('',#6991,#6986,#442,.T.);
#8606=EDGE_CURVE('',#6989,#6985,#443,.T.);
#8607=EDGE_CURVE('',#6988,#6992,#444,.T.);
#8608=EDGE_CURVE('',#6992,#6993,#445,.T.);
#8609=EDGE_CURVE('',#6994,#6993,#4176,.T.);
#8610=EDGE_CURVE('',#6995,#6994,#446,.T.);
#8611=EDGE_CURVE('',#6990,#6995,#447,.T.);
#8612=EDGE_CURVE('',#6993,#6996,#448,.T.);
#8613=EDGE_CURVE('',#6996,#6997,#449,.T.);
#8614=EDGE_CURVE('',#6998,#6997,#4177,.T.);
#8615=EDGE_CURVE('',#6999,#6998,#450,.T.);
#8616=EDGE_CURVE('',#6994,#6999,#451,.T.);
#8617=EDGE_CURVE('',#6997,#7000,#452,.T.);
#8618=EDGE_CURVE('',#7000,#6979,#453,.T.);
#8619=EDGE_CURVE('',#7001,#6978,#454,.T.);
#8620=EDGE_CURVE('',#6998,#7001,#455,.T.);
#8621=EDGE_CURVE('',#7000,#6980,#907,.T.);
#8622=EDGE_CURVE('',#6996,#7000,#908,.T.);
#8623=EDGE_CURVE('',#6992,#6996,#909,.T.);
#8624=EDGE_CURVE('',#6989,#6992,#910,.T.);
#8625=EDGE_CURVE('',#6989,#6984,#911,.T.);
#8626=EDGE_CURVE('',#6980,#6984,#912,.T.);
#8627=EDGE_CURVE('',#7001,#6999,#913,.T.);
#8628=EDGE_CURVE('',#6983,#7001,#914,.T.);
#8629=EDGE_CURVE('',#6987,#6983,#915,.T.);
#8630=EDGE_CURVE('',#6991,#6987,#916,.T.);
#8631=EDGE_CURVE('',#6995,#6991,#917,.T.);
#8632=EDGE_CURVE('',#6999,#6995,#918,.T.);
#8633=EDGE_CURVE('',#7002,#7003,#4178,.T.);
#8634=EDGE_CURVE('',#7004,#7002,#456,.T.);
#8635=EDGE_CURVE('',#7005,#7004,#919,.T.);
#8636=EDGE_CURVE('',#7005,#7003,#457,.T.);
#8637=EDGE_CURVE('',#7006,#7007,#4179,.T.);
#8638=EDGE_CURVE('',#7002,#7006,#458,.T.);
#8639=EDGE_CURVE('',#7003,#7007,#459,.T.);
#8640=EDGE_CURVE('',#7008,#7009,#4180,.T.);
#8641=EDGE_CURVE('',#7006,#7008,#460,.T.);
#8642=EDGE_CURVE('',#7007,#7009,#461,.T.);
#8643=EDGE_CURVE('',#7010,#7011,#4181,.T.);
#8644=EDGE_CURVE('',#7008,#7010,#462,.T.);
#8645=EDGE_CURVE('',#7009,#7011,#463,.T.);
#8646=EDGE_CURVE('',#7012,#7013,#4182,.T.);
#8647=EDGE_CURVE('',#7010,#7012,#464,.T.);
#8648=EDGE_CURVE('',#7011,#7013,#465,.T.);
#8649=EDGE_CURVE('',#7014,#7015,#4183,.T.);
#8650=EDGE_CURVE('',#7012,#7014,#466,.T.);
#8651=EDGE_CURVE('',#7013,#7015,#467,.T.);
#8652=EDGE_CURVE('',#7016,#7017,#4184,.T.);
#8653=EDGE_CURVE('',#7014,#7016,#468,.T.);
#8654=EDGE_CURVE('',#7015,#7017,#469,.T.);
#8655=EDGE_CURVE('',#7018,#7019,#4185,.T.);
#8656=EDGE_CURVE('',#7016,#7018,#470,.T.);
#8657=EDGE_CURVE('',#7017,#7019,#471,.T.);
#8658=EDGE_CURVE('',#7020,#7021,#4186,.T.);
#8659=EDGE_CURVE('',#7018,#7020,#472,.T.);
#8660=EDGE_CURVE('',#7019,#7021,#473,.T.);
#8661=EDGE_CURVE('',#7022,#7023,#4187,.T.);
#8662=EDGE_CURVE('',#7020,#7022,#474,.T.);
#8663=EDGE_CURVE('',#7021,#7023,#475,.T.);
#8664=EDGE_CURVE('',#7024,#7025,#4188,.T.);
#8665=EDGE_CURVE('',#7022,#7024,#476,.T.);
#8666=EDGE_CURVE('',#7023,#7025,#477,.T.);
#8667=EDGE_CURVE('',#7026,#7027,#4189,.T.);
#8668=EDGE_CURVE('',#7024,#7026,#478,.T.);
#8669=EDGE_CURVE('',#7025,#7027,#479,.T.);
#8670=EDGE_CURVE('',#7028,#7029,#4190,.T.);
#8671=EDGE_CURVE('',#7026,#7028,#480,.T.);
#8672=EDGE_CURVE('',#7027,#7029,#481,.T.);
#8673=EDGE_CURVE('',#7030,#7031,#4191,.T.);
#8674=EDGE_CURVE('',#7028,#7030,#482,.T.);
#8675=EDGE_CURVE('',#7029,#7031,#483,.T.);
#8676=EDGE_CURVE('',#7032,#7033,#4192,.T.);
#8677=EDGE_CURVE('',#7030,#7032,#484,.T.);
#8678=EDGE_CURVE('',#7031,#7033,#485,.T.);
#8679=EDGE_CURVE('',#7034,#7035,#4193,.T.);
#8680=EDGE_CURVE('',#7032,#7034,#486,.T.);
#8681=EDGE_CURVE('',#7033,#7035,#487,.T.);
#8682=EDGE_CURVE('',#7036,#7037,#4194,.T.);
#8683=EDGE_CURVE('',#7034,#7036,#488,.T.);
#8684=EDGE_CURVE('',#7035,#7037,#489,.T.);
#8685=EDGE_CURVE('',#7038,#7039,#4195,.T.);
#8686=EDGE_CURVE('',#7036,#7038,#490,.T.);
#8687=EDGE_CURVE('',#7037,#7039,#491,.T.);
#8688=EDGE_CURVE('',#7040,#7041,#4196,.T.);
#8689=EDGE_CURVE('',#7038,#7040,#492,.T.);
#8690=EDGE_CURVE('',#7039,#7041,#493,.T.);
#8691=EDGE_CURVE('',#7042,#7043,#4197,.T.);
#8692=EDGE_CURVE('',#7040,#7042,#494,.T.);
#8693=EDGE_CURVE('',#7041,#7043,#495,.T.);
#8694=EDGE_CURVE('',#7044,#7045,#4198,.T.);
#8695=EDGE_CURVE('',#7042,#7044,#496,.T.);
#8696=EDGE_CURVE('',#7043,#7045,#497,.T.);
#8697=EDGE_CURVE('',#7046,#7047,#4199,.T.);
#8698=EDGE_CURVE('',#7044,#7046,#498,.T.);
#8699=EDGE_CURVE('',#7045,#7047,#499,.T.);
#8700=EDGE_CURVE('',#7048,#7049,#4200,.T.);
#8701=EDGE_CURVE('',#7048,#7050,#317,.T.);
#8702=EDGE_CURVE('',#7050,#7051,#4201,.T.);
#8703=EDGE_CURVE('',#7051,#7052,#318,.T.);
#8704=EDGE_CURVE('',#7052,#7053,#319,.T.);
#8705=EDGE_CURVE('',#7053,#7054,#320,.T.);
#8706=EDGE_CURVE('',#7054,#7055,#321,.T.);
#8707=EDGE_CURVE('',#7055,#7056,#322,.T.);
#8708=EDGE_CURVE('',#7056,#7051,#323,.T.);
#8709=EDGE_CURVE('',#7050,#7057,#324,.T.);
#8710=EDGE_CURVE('',#7057,#7058,#4202,.T.);
#8711=EDGE_CURVE('',#7049,#7058,#325,.F.);
#8712=EDGE_CURVE('',#7059,#7060,#4203,.T.);
#8713=EDGE_CURVE('',#7059,#7048,#326,.T.);
#8714=EDGE_CURVE('',#7060,#7049,#327,.F.);
#8715=EDGE_CURVE('',#7061,#7062,#4204,.T.);
#8716=EDGE_CURVE('',#7061,#7059,#328,.T.);
#8717=EDGE_CURVE('',#7062,#7060,#329,.F.);
#8718=EDGE_CURVE('',#7063,#7064,#4205,.T.);
#8719=EDGE_CURVE('',#7063,#7061,#330,.T.);
#8720=EDGE_CURVE('',#7064,#7062,#331,.F.);
#8721=EDGE_CURVE('',#7065,#7066,#4206,.T.);
#8722=EDGE_CURVE('',#7065,#7063,#332,.T.);
#8723=EDGE_CURVE('',#7066,#7064,#333,.F.);
#8724=EDGE_CURVE('',#7067,#7068,#4207,.T.);
#8725=EDGE_CURVE('',#7067,#7065,#334,.T.);
#8726=EDGE_CURVE('',#7068,#7066,#335,.F.);
#8727=EDGE_CURVE('',#7069,#7070,#4208,.T.);
#8728=EDGE_CURVE('',#7069,#7067,#336,.T.);
#8729=EDGE_CURVE('',#7070,#7068,#337,.F.);
#8730=EDGE_CURVE('',#7071,#7072,#4209,.T.);
#8731=EDGE_CURVE('',#7071,#7069,#338,.T.);
#8732=EDGE_CURVE('',#7072,#7070,#339,.F.);
#8733=EDGE_CURVE('',#7073,#7074,#4210,.T.);
#8734=EDGE_CURVE('',#7073,#7071,#340,.T.);
#8735=EDGE_CURVE('',#7074,#7072,#341,.F.);
#8736=EDGE_CURVE('',#7075,#7076,#4211,.T.);
#8737=EDGE_CURVE('',#7075,#7073,#342,.T.);
#8738=EDGE_CURVE('',#7076,#7074,#343,.F.);
#8739=EDGE_CURVE('',#7077,#7078,#4212,.T.);
#8740=EDGE_CURVE('',#7077,#7075,#344,.T.);
#8741=EDGE_CURVE('',#7078,#7076,#345,.F.);
#8742=EDGE_CURVE('',#7079,#7080,#4213,.T.);
#8743=EDGE_CURVE('',#7079,#7077,#346,.T.);
#8744=EDGE_CURVE('',#7080,#7078,#347,.F.);
#8745=EDGE_CURVE('',#7081,#7082,#4214,.T.);
#8746=EDGE_CURVE('',#7081,#7079,#348,.T.);
#8747=EDGE_CURVE('',#7082,#7080,#349,.F.);
#8748=EDGE_CURVE('',#7083,#7084,#4215,.T.);
#8749=EDGE_CURVE('',#7083,#7081,#350,.T.);
#8750=EDGE_CURVE('',#7084,#7082,#351,.F.);
#8751=EDGE_CURVE('',#7085,#7086,#4216,.T.);
#8752=EDGE_CURVE('',#7085,#7083,#352,.T.);
#8753=EDGE_CURVE('',#7086,#7084,#353,.F.);
#8754=EDGE_CURVE('',#7087,#7088,#4217,.T.);
#8755=EDGE_CURVE('',#7087,#7085,#354,.T.);
#8756=EDGE_CURVE('',#7088,#7086,#355,.F.);
#8757=EDGE_CURVE('',#7089,#7090,#4218,.T.);
#8758=EDGE_CURVE('',#7089,#7087,#356,.T.);
#8759=EDGE_CURVE('',#7090,#7088,#357,.F.);
#8760=EDGE_CURVE('',#7091,#7092,#4219,.T.);
#8761=EDGE_CURVE('',#7091,#7089,#358,.T.);
#8762=EDGE_CURVE('',#7092,#7090,#359,.F.);
#8763=EDGE_CURVE('',#7093,#7094,#4220,.T.);
#8764=EDGE_CURVE('',#7093,#7091,#360,.T.);
#8765=EDGE_CURVE('',#7094,#7092,#361,.F.);
#8766=EDGE_CURVE('',#7095,#7096,#4221,.T.);
#8767=EDGE_CURVE('',#7095,#7093,#362,.T.);
#8768=EDGE_CURVE('',#7096,#7094,#363,.F.);
#8769=EDGE_CURVE('',#7097,#7098,#4222,.T.);
#8770=EDGE_CURVE('',#7097,#7099,#920,.T.);
#8771=EDGE_CURVE('',#7099,#7095,#364,.T.);
#8772=EDGE_CURVE('',#7098,#7096,#365,.F.);
#8773=EDGE_CURVE('',#7100,#7101,#921,.T.);
#8774=EDGE_CURVE('',#7100,#7102,#922,.T.);
#8775=EDGE_CURVE('',#7103,#7102,#923,.T.);
#8776=EDGE_CURVE('',#7101,#7103,#924,.T.);
#8777=EDGE_CURVE('',#7104,#7105,#925,.T.);
#8778=EDGE_CURVE('',#7104,#7106,#926,.T.);
#8779=EDGE_CURVE('',#7107,#7106,#927,.T.);
#8780=EDGE_CURVE('',#7105,#7107,#928,.T.);
#8781=EDGE_CURVE('',#7108,#7108,#929,.T.);
#8782=EDGE_CURVE('',#7108,#7109,#4223,.T.);
#8783=EDGE_CURVE('',#7109,#7109,#930,.T.);
#8784=EDGE_CURVE('',#7106,#7100,#366,.T.);
#8785=EDGE_CURVE('',#7101,#7107,#367,.T.);
#8786=EDGE_CURVE('',#7004,#7099,#368,.T.);
#8787=EDGE_CURVE('',#7110,#7097,#931,.T.);
#8788=EDGE_CURVE('',#7110,#7111,#369,.T.);
#8789=EDGE_CURVE('',#7111,#7112,#4224,.T.);
#8790=EDGE_CURVE('',#7112,#7112,#932,.T.);
#8791=EDGE_CURVE('',#7111,#7005,#370,.T.);
#8792=EDGE_CURVE('',#7110,#7098,#371,.F.);
#8793=EDGE_CURVE('',#7105,#7113,#372,.T.);
#8794=EDGE_CURVE('',#7113,#7051,#373,.T.);
#8795=EDGE_CURVE('',#7051,#7114,#374,.T.);
#8796=EDGE_CURVE('',#7114,#7104,#375,.T.);
#8797=EDGE_CURVE('',#7102,#7115,#376,.T.);
#8798=EDGE_CURVE('',#7115,#7054,#377,.T.);
#8799=EDGE_CURVE('',#7054,#7116,#378,.T.);
#8800=EDGE_CURVE('',#7116,#7103,#379,.T.);
#8801=EDGE_CURVE('',#7058,#7117,#4225,.T.);
#8802=EDGE_CURVE('',#7118,#7057,#4226,.T.);
#8803=EDGE_CURVE('',#7117,#7118,#4227,.T.);
#8804=EDGE_CURVE('',#7047,#7117,#500,.T.);
#8805=EDGE_CURVE('',#7046,#7118,#501,.T.);
#8806=EDGE_CURVE('',#7051,#7119,#380,.T.);
#8807=EDGE_CURVE('',#7052,#7119,#933,.T.);
#8808=EDGE_CURVE('',#7119,#7107,#381,.T.);
#8809=EDGE_CURVE('',#7101,#7120,#382,.T.);
#8810=EDGE_CURVE('',#7053,#7120,#934,.T.);
#8811=EDGE_CURVE('',#7120,#7054,#383,.T.);
#8812=EDGE_CURVE('',#7054,#7121,#384,.T.);
#8813=EDGE_CURVE('',#7055,#7121,#935,.T.);
#8814=EDGE_CURVE('',#7121,#7100,#385,.T.);
#8815=EDGE_CURVE('',#7106,#7122,#386,.T.);
#8816=EDGE_CURVE('',#7056,#7122,#936,.T.);
#8817=EDGE_CURVE('',#7122,#7051,#387,.T.);
#8818=EDGE_CURVE('',#7114,#7122,#937,.T.);
#8819=EDGE_CURVE('',#7113,#7119,#938,.T.);
#8820=EDGE_CURVE('',#7121,#7115,#939,.T.);
#8821=EDGE_CURVE('',#7120,#7116,#940,.T.);
#8822=EDGE_CURVE('',#7123,#7124,#4228,.T.);
#8823=EDGE_CURVE('',#7124,#7125,#502,.T.);
#8824=EDGE_CURVE('',#7125,#7126,#941,.T.);
#8825=EDGE_CURVE('',#7123,#7126,#503,.T.);
#8826=EDGE_CURVE('',#7127,#7128,#4229,.T.);
#8827=EDGE_CURVE('',#7128,#7124,#504,.T.);
#8828=EDGE_CURVE('',#7127,#7123,#505,.T.);
#8829=EDGE_CURVE('',#7129,#7130,#4230,.T.);
#8830=EDGE_CURVE('',#7130,#7128,#506,.T.);
#8831=EDGE_CURVE('',#7129,#7127,#507,.T.);
#8832=EDGE_CURVE('',#7131,#7132,#4231,.T.);
#8833=EDGE_CURVE('',#7132,#7130,#508,.T.);
#8834=EDGE_CURVE('',#7131,#7129,#509,.T.);
#8835=EDGE_CURVE('',#7133,#7134,#4232,.T.);
#8836=EDGE_CURVE('',#7135,#7133,#510,.T.);
#8837=EDGE_CURVE('',#7135,#7136,#942,.T.);
#8838=EDGE_CURVE('',#7136,#7134,#511,.T.);
#8839=EDGE_CURVE('',#7137,#7138,#4233,.T.);
#8840=EDGE_CURVE('',#7139,#7138,#943,.T.);
#8841=EDGE_CURVE('',#7137,#7139,#388,.F.);
#8842=EDGE_CURVE('',#7140,#7141,#4234,.T.);
#8843=EDGE_CURVE('',#7141,#7142,#389,.T.);
#8844=EDGE_CURVE('',#7138,#7142,#944,.T.);
#8845=EDGE_CURVE('',#7140,#7137,#390,.F.);
#8846=EDGE_CURVE('',#7143,#7144,#4235,.T.);
#8847=EDGE_CURVE('',#7144,#7141,#391,.T.);
#8848=EDGE_CURVE('',#7143,#7140,#392,.F.);
#8849=EDGE_CURVE('',#7145,#7146,#4236,.T.);
#8850=EDGE_CURVE('',#7146,#7144,#393,.T.);
#8851=EDGE_CURVE('',#7145,#7143,#394,.F.);
#8852=EDGE_CURVE('',#7147,#7148,#4237,.T.);
#8853=EDGE_CURVE('',#7148,#7146,#395,.T.);
#8854=EDGE_CURVE('',#7147,#7145,#396,.F.);
#8855=EDGE_CURVE('',#7149,#7150,#4238,.T.);
#8856=EDGE_CURVE('',#7151,#7149,#397,.F.);
#8857=EDGE_CURVE('',#7151,#7152,#945,.T.);
#8858=EDGE_CURVE('',#7152,#7150,#398,.T.);
#8859=EDGE_CURVE('',#7153,#7153,#946,.T.);
#8860=EDGE_CURVE('',#7153,#7154,#4239,.T.);
#8861=EDGE_CURVE('',#7154,#7154,#947,.T.);
#8862=EDGE_CURVE('',#7155,#7156,#948,.T.);
#8863=EDGE_CURVE('',#7156,#7153,#4240,.T.);
#8864=EDGE_CURVE('',#7156,#7155,#949,.T.);
#8865=EDGE_CURVE('',#7155,#7157,#4241,.T.);
#8866=EDGE_CURVE('',#7158,#7157,#950,.T.);
#8867=EDGE_CURVE('',#7159,#7158,#668,.T.);
#8868=EDGE_CURVE('',#7160,#7159,#399,.T.);
#8869=EDGE_CURVE('',#7160,#7161,#512,.F.);
#8870=EDGE_CURVE('',#7162,#7161,#400,.T.);
#8871=EDGE_CURVE('',#7163,#7162,#669,.T.);
#8872=EDGE_CURVE('',#7157,#7163,#951,.T.);
#8873=EDGE_CURVE('',#7150,#7148,#401,.T.);
#8874=EDGE_CURVE('',#7149,#7147,#402,.F.);
#8875=EDGE_CURVE('',#7162,#7164,#513,.T.);
#8876=EDGE_CURVE('',#7161,#7164,#952,.T.);
#8877=EDGE_CURVE('',#7165,#7163,#670,.T.);
#8878=EDGE_CURVE('',#7166,#7164,#4242,.T.);
#8879=EDGE_CURVE('',#7166,#7167,#514,.T.);
#8880=EDGE_CURVE('',#7167,#7168,#4243,.T.);
#8881=EDGE_CURVE('',#7168,#7169,#515,.T.);
#8882=EDGE_CURVE('',#7169,#7170,#4244,.T.);
#8883=EDGE_CURVE('',#7170,#7171,#516,.T.);
#8884=EDGE_CURVE('',#7165,#7171,#4245,.T.);
#8885=EDGE_CURVE('',#7172,#7159,#403,.T.);
#8886=EDGE_CURVE('',#7158,#7165,#671,.T.);
#8887=EDGE_CURVE('',#7171,#7173,#517,.T.);
#8888=EDGE_CURVE('',#7173,#7174,#4246,.T.);
#8889=EDGE_CURVE('',#7174,#7175,#518,.T.);
#8890=EDGE_CURVE('',#7176,#7175,#4247,.T.);
#8891=EDGE_CURVE('',#7176,#7177,#519,.T.);
#8892=EDGE_CURVE('',#7172,#7177,#4248,.T.);
#8893=EDGE_CURVE('',#7172,#7160,#953,.T.);
#8894=EDGE_CURVE('',#7178,#7177,#954,.T.);
#8895=EDGE_CURVE('',#7178,#7179,#4249,.T.);
#8896=EDGE_CURVE('',#7180,#7179,#955,.T.);
#8897=EDGE_CURVE('',#7180,#7181,#4250,.T.);
#8898=EDGE_CURVE('',#7182,#7181,#956,.T.);
#8899=EDGE_CURVE('',#7182,#7183,#4251,.T.);
#8900=EDGE_CURVE('',#7184,#7183,#957,.T.);
#8901=EDGE_CURVE('',#7184,#7185,#4252,.T.);
#8902=EDGE_CURVE('',#7166,#7185,#958,.T.);
#8903=EDGE_CURVE('',#7136,#7151,#404,.T.);
#8904=EDGE_CURVE('',#7152,#7135,#405,.T.);
#8905=EDGE_CURVE('',#7169,#7186,#959,.T.);
#8906=EDGE_CURVE('',#7187,#7186,#4253,.T.);
#8907=EDGE_CURVE('',#7187,#7188,#960,.T.);
#8908=EDGE_CURVE('',#7189,#7188,#4254,.T.);
#8909=EDGE_CURVE('',#7189,#7190,#961,.T.);
#8910=EDGE_CURVE('',#7191,#7190,#4255,.T.);
#8911=EDGE_CURVE('',#7191,#7192,#962,.T.);
#8912=EDGE_CURVE('',#7193,#7192,#4256,.T.);
#8913=EDGE_CURVE('',#7193,#7174,#963,.T.);
#8914=EDGE_CURVE('',#7173,#7170,#964,.T.);
#8915=EDGE_CURVE('',#7126,#7142,#406,.T.);
#8916=EDGE_CURVE('',#7139,#7125,#407,.T.);
#8917=EDGE_CURVE('',#7194,#7195,#4257,.T.);
#8918=EDGE_CURVE('',#7194,#7179,#520,.T.);
#8919=EDGE_CURVE('',#7178,#7176,#521,.T.);
#8920=EDGE_CURVE('',#7175,#7193,#522,.T.);
#8921=EDGE_CURVE('',#7192,#7195,#523,.T.);
#8922=EDGE_CURVE('',#7196,#7197,#4258,.T.);
#8923=EDGE_CURVE('',#7196,#7181,#524,.T.);
#8924=EDGE_CURVE('',#7180,#7194,#525,.T.);
#8925=EDGE_CURVE('',#7195,#7191,#526,.T.);
#8926=EDGE_CURVE('',#7190,#7197,#527,.T.);
#8927=EDGE_CURVE('',#7198,#7199,#4259,.T.);
#8928=EDGE_CURVE('',#7198,#7183,#528,.T.);
#8929=EDGE_CURVE('',#7182,#7196,#529,.T.);
#8930=EDGE_CURVE('',#7197,#7189,#530,.T.);
#8931=EDGE_CURVE('',#7188,#7199,#531,.T.);
#8932=EDGE_CURVE('',#7167,#7185,#532,.T.);
#8933=EDGE_CURVE('',#7184,#7198,#533,.T.);
#8934=EDGE_CURVE('',#7199,#7187,#534,.T.);
#8935=EDGE_CURVE('',#7186,#7168,#535,.T.);
#8936=EDGE_CURVE('',#7133,#7131,#536,.T.);
#8937=EDGE_CURVE('',#7134,#7132,#537,.T.);
#8938=EDGE_CURVE('',#7200,#7200,#965,.T.);
#8939=EDGE_CURVE('',#7200,#7201,#4260,.T.);
#8940=EDGE_CURVE('',#7201,#7201,#966,.T.);
#8941=EDGE_CURVE('',#7202,#7202,#967,.T.);
#8942=EDGE_CURVE('',#7202,#7203,#4261,.T.);
#8943=EDGE_CURVE('',#7203,#7203,#968,.T.);
#8944=EDGE_CURVE('',#7204,#7205,#4262,.T.);
#8945=EDGE_CURVE('',#7206,#7205,#4263,.T.);
#8946=EDGE_CURVE('',#7207,#7206,#4264,.T.);
#8947=EDGE_CURVE('',#7207,#7204,#4265,.T.);
#8948=EDGE_CURVE('',#7205,#7208,#4266,.T.);
#8949=EDGE_CURVE('',#7209,#7208,#4267,.T.);
#8950=EDGE_CURVE('',#7206,#7209,#4268,.T.);
#8951=EDGE_CURVE('',#7208,#7210,#4269,.T.);
#8952=EDGE_CURVE('',#7211,#7210,#4270,.T.);
#8953=EDGE_CURVE('',#7209,#7211,#4271,.T.);
#8954=EDGE_CURVE('',#7210,#7204,#4272,.T.);
#8955=EDGE_CURVE('',#7211,#7207,#4273,.T.);
#8956=EDGE_CURVE('',#7212,#7212,#969,.T.);
#8957=EDGE_CURVE('',#7212,#7213,#4274,.T.);
#8958=EDGE_CURVE('',#7213,#7213,#970,.T.);
#8959=EDGE_CURVE('',#7214,#7215,#4275,.T.);
#8960=EDGE_CURVE('',#7215,#7216,#4276,.T.);
#8961=EDGE_CURVE('',#7216,#7217,#4277,.T.);
#8962=EDGE_CURVE('',#7217,#7218,#4278,.T.);
#8963=EDGE_CURVE('',#7218,#7219,#971,.T.);
#8964=EDGE_CURVE('',#7219,#7214,#4279,.T.);
#8965=EDGE_CURVE('',#7220,#7221,#4280,.T.);
#8966=EDGE_CURVE('',#7222,#7220,#4281,.T.);
#8967=EDGE_CURVE('',#7223,#7222,#972,.T.);
#8968=EDGE_CURVE('',#7224,#7223,#4282,.T.);
#8969=EDGE_CURVE('',#7225,#7224,#4283,.T.);
#8970=EDGE_CURVE('',#7221,#7225,#4284,.T.);
#8971=EDGE_CURVE('',#7215,#7221,#4285,.T.);
#8972=EDGE_CURVE('',#7214,#7220,#4286,.T.);
#8973=EDGE_CURVE('',#7216,#7225,#4287,.T.);
#8974=EDGE_CURVE('',#7217,#7224,#4288,.T.);
#8975=EDGE_CURVE('',#7218,#7223,#4289,.T.);
#8976=EDGE_CURVE('',#7219,#7222,#4290,.T.);
#8977=EDGE_CURVE('',#7226,#7226,#973,.T.);
#8978=EDGE_CURVE('',#7226,#7227,#4291,.T.);
#8979=EDGE_CURVE('',#7227,#7227,#974,.T.);
#8980=EDGE_CURVE('',#7228,#7229,#4292,.T.);
#8981=EDGE_CURVE('',#7230,#7228,#4293,.T.);
#8982=EDGE_CURVE('',#7231,#7230,#975,.T.);
#8983=EDGE_CURVE('',#7232,#7231,#4294,.T.);
#8984=EDGE_CURVE('',#7233,#7232,#4295,.T.);
#8985=EDGE_CURVE('',#7229,#7233,#4296,.T.);
#8986=EDGE_CURVE('',#7234,#7235,#4297,.T.);
#8987=EDGE_CURVE('',#7235,#7236,#4298,.T.);
#8988=EDGE_CURVE('',#7236,#7237,#4299,.T.);
#8989=EDGE_CURVE('',#7237,#7238,#4300,.T.);
#8990=EDGE_CURVE('',#7238,#7239,#976,.T.);
#8991=EDGE_CURVE('',#7239,#7234,#4301,.T.);
#8992=EDGE_CURVE('',#7228,#7234,#4302,.T.);
#8993=EDGE_CURVE('',#7229,#7235,#4303,.T.);
#8994=EDGE_CURVE('',#7233,#7236,#4304,.T.);
#8995=EDGE_CURVE('',#7232,#7237,#4305,.T.);
#8996=EDGE_CURVE('',#7231,#7238,#4306,.T.);
#8997=EDGE_CURVE('',#7230,#7239,#4307,.T.);
#8998=EDGE_CURVE('',#7240,#7240,#977,.T.);
#8999=EDGE_CURVE('',#7240,#7241,#4308,.T.);
#9000=EDGE_CURVE('',#7241,#7241,#978,.T.);
#9001=EDGE_CURVE('',#7242,#7242,#979,.T.);
#9002=EDGE_CURVE('',#7242,#7243,#4309,.T.);
#9003=EDGE_CURVE('',#7243,#7243,#980,.T.);
#9004=EDGE_CURVE('',#7244,#7244,#981,.T.);
#9005=EDGE_CURVE('',#7244,#7245,#4310,.T.);
#9006=EDGE_CURVE('',#7245,#7245,#982,.T.);
#9007=EDGE_CURVE('',#7246,#7246,#983,.T.);
#9008=EDGE_CURVE('',#7246,#7247,#4311,.T.);
#9009=EDGE_CURVE('',#7247,#7247,#984,.T.);
#9010=EDGE_CURVE('',#7248,#7248,#985,.T.);
#9011=EDGE_CURVE('',#7248,#7249,#4312,.T.);
#9012=EDGE_CURVE('',#7249,#7249,#986,.T.);
#9013=EDGE_CURVE('',#7250,#7251,#4313,.T.);
#9014=EDGE_CURVE('',#7251,#7252,#4314,.T.);
#9015=EDGE_CURVE('',#7252,#7253,#4315,.T.);
#9016=EDGE_CURVE('',#7253,#7254,#4316,.T.);
#9017=EDGE_CURVE('',#7254,#7255,#4317,.T.);
#9018=EDGE_CURVE('',#7255,#7256,#4318,.T.);
#9019=EDGE_CURVE('',#7256,#7257,#4319,.T.);
#9020=EDGE_CURVE('',#7257,#7250,#4320,.T.);
#9021=EDGE_CURVE('',#7258,#7259,#4321,.T.);
#9022=EDGE_CURVE('',#7260,#7258,#4322,.T.);
#9023=EDGE_CURVE('',#7261,#7260,#4323,.T.);
#9024=EDGE_CURVE('',#7262,#7261,#4324,.T.);
#9025=EDGE_CURVE('',#7263,#7262,#4325,.T.);
#9026=EDGE_CURVE('',#7264,#7263,#4326,.T.);
#9027=EDGE_CURVE('',#7265,#7264,#4327,.T.);
#9028=EDGE_CURVE('',#7259,#7265,#4328,.T.);
#9029=EDGE_CURVE('',#7251,#7259,#4329,.T.);
#9030=EDGE_CURVE('',#7250,#7258,#4330,.T.);
#9031=EDGE_CURVE('',#7252,#7265,#4331,.T.);
#9032=EDGE_CURVE('',#7253,#7264,#4332,.T.);
#9033=EDGE_CURVE('',#7254,#7263,#4333,.T.);
#9034=EDGE_CURVE('',#7255,#7262,#4334,.T.);
#9035=EDGE_CURVE('',#7256,#7261,#4335,.T.);
#9036=EDGE_CURVE('',#7257,#7260,#4336,.T.);
#9037=EDGE_CURVE('',#7266,#7267,#4337,.T.);
#9038=EDGE_CURVE('',#7268,#7267,#4338,.T.);
#9039=EDGE_CURVE('',#7269,#7268,#4339,.T.);
#9040=EDGE_CURVE('',#7269,#7266,#4340,.T.);
#9041=EDGE_CURVE('',#7267,#7270,#4341,.T.);
#9042=EDGE_CURVE('',#7271,#7270,#4342,.T.);
#9043=EDGE_CURVE('',#7268,#7271,#4343,.T.);
#9044=EDGE_CURVE('',#7270,#7272,#4344,.T.);
#9045=EDGE_CURVE('',#7273,#7272,#4345,.T.);
#9046=EDGE_CURVE('',#7271,#7273,#4346,.T.);
#9047=EDGE_CURVE('',#7272,#7266,#4347,.T.);
#9048=EDGE_CURVE('',#7273,#7269,#4348,.T.);
#9049=EDGE_CURVE('',#7274,#7275,#4349,.T.);
#9050=EDGE_CURVE('',#7276,#7275,#4350,.T.);
#9051=EDGE_CURVE('',#7277,#7276,#4351,.T.);
#9052=EDGE_CURVE('',#7277,#7274,#4352,.T.);
#9053=EDGE_CURVE('',#7275,#7278,#4353,.T.);
#9054=EDGE_CURVE('',#7279,#7278,#4354,.T.);
#9055=EDGE_CURVE('',#7276,#7279,#4355,.T.);
#9056=EDGE_CURVE('',#7278,#7280,#4356,.T.);
#9057=EDGE_CURVE('',#7281,#7280,#4357,.T.);
#9058=EDGE_CURVE('',#7279,#7281,#4358,.T.);
#9059=EDGE_CURVE('',#7280,#7274,#4359,.T.);
#9060=EDGE_CURVE('',#7281,#7277,#4360,.T.);
#9061=EDGE_CURVE('',#7282,#7283,#4361,.T.);
#9062=EDGE_CURVE('',#7284,#7283,#4362,.T.);
#9063=EDGE_CURVE('',#7285,#7284,#4363,.T.);
#9064=EDGE_CURVE('',#7285,#7282,#4364,.T.);
#9065=EDGE_CURVE('',#7283,#7286,#4365,.T.);
#9066=EDGE_CURVE('',#7287,#7286,#4366,.T.);
#9067=EDGE_CURVE('',#7284,#7287,#4367,.T.);
#9068=EDGE_CURVE('',#7286,#7288,#4368,.T.);
#9069=EDGE_CURVE('',#7289,#7288,#4369,.T.);
#9070=EDGE_CURVE('',#7287,#7289,#4370,.T.);
#9071=EDGE_CURVE('',#7288,#7290,#4371,.T.);
#9072=EDGE_CURVE('',#7291,#7290,#4372,.T.);
#9073=EDGE_CURVE('',#7289,#7291,#4373,.T.);
#9074=EDGE_CURVE('',#7290,#7292,#4374,.T.);
#9075=EDGE_CURVE('',#7293,#7292,#4375,.T.);
#9076=EDGE_CURVE('',#7291,#7293,#4376,.T.);
#9077=EDGE_CURVE('',#7292,#7282,#4377,.T.);
#9078=EDGE_CURVE('',#7293,#7285,#4378,.T.);
#9079=EDGE_CURVE('',#7294,#7294,#987,.T.);
#9080=EDGE_CURVE('',#7294,#7295,#4379,.T.);
#9081=EDGE_CURVE('',#7295,#7295,#988,.T.);
#9082=EDGE_CURVE('',#7296,#7296,#989,.T.);
#9083=EDGE_CURVE('',#7296,#7297,#4380,.T.);
#9084=EDGE_CURVE('',#7297,#7297,#990,.T.);
#9085=EDGE_CURVE('',#7298,#7298,#991,.T.);
#9086=EDGE_CURVE('',#7298,#7299,#4381,.T.);
#9087=EDGE_CURVE('',#7299,#7299,#992,.T.);
#9088=EDGE_CURVE('',#7300,#7301,#4382,.T.);
#9089=EDGE_CURVE('',#7301,#7302,#4383,.T.);
#9090=EDGE_CURVE('',#7302,#7303,#4384,.T.);
#9091=EDGE_CURVE('',#7303,#7300,#4385,.T.);
#9092=EDGE_CURVE('',#7304,#7305,#4386,.T.);
#9093=EDGE_CURVE('',#7306,#7304,#4387,.T.);
#9094=EDGE_CURVE('',#7307,#7306,#4388,.T.);
#9095=EDGE_CURVE('',#7305,#7307,#4389,.T.);
#9096=EDGE_CURVE('',#7301,#7305,#4390,.T.);
#9097=EDGE_CURVE('',#7300,#7304,#4391,.T.);
#9098=EDGE_CURVE('',#7302,#7307,#4392,.T.);
#9099=EDGE_CURVE('',#7303,#7306,#4393,.T.);
#9100=EDGE_CURVE('',#7308,#7308,#993,.T.);
#9101=EDGE_CURVE('',#7308,#7309,#4394,.T.);
#9102=EDGE_CURVE('',#7309,#7309,#994,.T.);
#9103=EDGE_CURVE('',#7310,#7310,#995,.T.);
#9104=EDGE_CURVE('',#7310,#7311,#4395,.T.);
#9105=EDGE_CURVE('',#7311,#7311,#996,.T.);
#9106=EDGE_CURVE('',#7312,#7312,#997,.T.);
#9107=EDGE_CURVE('',#7312,#7313,#4396,.T.);
#9108=EDGE_CURVE('',#7313,#7313,#998,.T.);
#9109=EDGE_CURVE('',#7314,#7315,#4397,.T.);
#9110=EDGE_CURVE('',#7315,#7316,#4398,.T.);
#9111=EDGE_CURVE('',#7316,#7317,#4399,.T.);
#9112=EDGE_CURVE('',#7317,#7314,#4400,.T.);
#9113=EDGE_CURVE('',#7318,#7319,#4401,.T.);
#9114=EDGE_CURVE('',#7320,#7318,#4402,.T.);
#9115=EDGE_CURVE('',#7321,#7320,#4403,.T.);
#9116=EDGE_CURVE('',#7319,#7321,#4404,.T.);
#9117=EDGE_CURVE('',#7315,#7319,#4405,.T.);
#9118=EDGE_CURVE('',#7314,#7318,#4406,.T.);
#9119=EDGE_CURVE('',#7316,#7321,#4407,.T.);
#9120=EDGE_CURVE('',#7317,#7320,#4408,.T.);
#9121=EDGE_CURVE('',#7322,#7322,#999,.T.);
#9122=EDGE_CURVE('',#7322,#7323,#4409,.T.);
#9123=EDGE_CURVE('',#7323,#7323,#1000,.T.);
#9124=EDGE_CURVE('',#7324,#7324,#1001,.T.);
#9125=EDGE_CURVE('',#7324,#7325,#4410,.T.);
#9126=EDGE_CURVE('',#7325,#7325,#1002,.T.);
#9127=EDGE_CURVE('',#7326,#7326,#1003,.T.);
#9128=EDGE_CURVE('',#7326,#7327,#4411,.T.);
#9129=EDGE_CURVE('',#7327,#7327,#1004,.T.);
#9130=EDGE_CURVE('',#7328,#7329,#4412,.T.);
#9131=EDGE_CURVE('',#7329,#7330,#4413,.T.);
#9132=EDGE_CURVE('',#7330,#7331,#4414,.T.);
#9133=EDGE_CURVE('',#7331,#7328,#4415,.T.);
#9134=EDGE_CURVE('',#7332,#7333,#4416,.T.);
#9135=EDGE_CURVE('',#7334,#7332,#4417,.T.);
#9136=EDGE_CURVE('',#7335,#7334,#4418,.T.);
#9137=EDGE_CURVE('',#7333,#7335,#4419,.T.);
#9138=EDGE_CURVE('',#7329,#7333,#4420,.T.);
#9139=EDGE_CURVE('',#7328,#7332,#4421,.T.);
#9140=EDGE_CURVE('',#7330,#7335,#4422,.T.);
#9141=EDGE_CURVE('',#7331,#7334,#4423,.T.);
#9142=EDGE_CURVE('',#7336,#7336,#1005,.T.);
#9143=EDGE_CURVE('',#7336,#7337,#4424,.T.);
#9144=EDGE_CURVE('',#7337,#7337,#1006,.T.);
#9145=EDGE_CURVE('',#7338,#7338,#1007,.T.);
#9146=EDGE_CURVE('',#7338,#7339,#4425,.T.);
#9147=EDGE_CURVE('',#7339,#7339,#1008,.T.);
#9148=EDGE_CURVE('',#7340,#7340,#1009,.T.);
#9149=EDGE_CURVE('',#7340,#7341,#4426,.T.);
#9150=EDGE_CURVE('',#7341,#7341,#1010,.T.);
#9151=EDGE_CURVE('',#7342,#7343,#4427,.T.);
#9152=EDGE_CURVE('',#7343,#7344,#4428,.T.);
#9153=EDGE_CURVE('',#7344,#7345,#4429,.T.);
#9154=EDGE_CURVE('',#7345,#7342,#4430,.T.);
#9155=EDGE_CURVE('',#7346,#7347,#4431,.T.);
#9156=EDGE_CURVE('',#7348,#7346,#4432,.T.);
#9157=EDGE_CURVE('',#7349,#7348,#4433,.T.);
#9158=EDGE_CURVE('',#7347,#7349,#4434,.T.);
#9159=EDGE_CURVE('',#7343,#7347,#4435,.T.);
#9160=EDGE_CURVE('',#7342,#7346,#4436,.T.);
#9161=EDGE_CURVE('',#7344,#7349,#4437,.T.);
#9162=EDGE_CURVE('',#7345,#7348,#4438,.T.);
#9163=EDGE_CURVE('',#7350,#7351,#4439,.T.);
#9164=EDGE_CURVE('',#7352,#7350,#4440,.T.);
#9165=EDGE_CURVE('',#7352,#7353,#4441,.T.);
#9166=EDGE_CURVE('',#7353,#7351,#4442,.T.);
#9167=EDGE_CURVE('',#7351,#7354,#4443,.T.);
#9168=EDGE_CURVE('',#7353,#7355,#4444,.T.);
#9169=EDGE_CURVE('',#7355,#7354,#4445,.T.);
#9170=EDGE_CURVE('',#7354,#7356,#4446,.T.);
#9171=EDGE_CURVE('',#7355,#7357,#4447,.T.);
#9172=EDGE_CURVE('',#7357,#7356,#4448,.T.);
#9173=EDGE_CURVE('',#7356,#7350,#4449,.T.);
#9174=EDGE_CURVE('',#7357,#7352,#4450,.T.);
#9175=EDGE_CURVE('',#7358,#7359,#4451,.T.);
#9176=EDGE_CURVE('',#7360,#7358,#4452,.T.);
#9177=EDGE_CURVE('',#7360,#7361,#4453,.T.);
#9178=EDGE_CURVE('',#7361,#7359,#4454,.T.);
#9179=EDGE_CURVE('',#7359,#7362,#4455,.T.);
#9180=EDGE_CURVE('',#7361,#7363,#4456,.T.);
#9181=EDGE_CURVE('',#7363,#7362,#4457,.T.);
#9182=EDGE_CURVE('',#7362,#7364,#4458,.T.);
#9183=EDGE_CURVE('',#7363,#7365,#4459,.T.);
#9184=EDGE_CURVE('',#7365,#7364,#4460,.T.);
#9185=EDGE_CURVE('',#7364,#7358,#4461,.T.);
#9186=EDGE_CURVE('',#7365,#7360,#4462,.T.);
#9187=EDGE_CURVE('',#7366,#7367,#4463,.T.);
#9188=EDGE_CURVE('',#7368,#7366,#4464,.T.);
#9189=EDGE_CURVE('',#7368,#7369,#4465,.T.);
#9190=EDGE_CURVE('',#7369,#7367,#4466,.T.);
#9191=EDGE_CURVE('',#7370,#7366,#4467,.T.);
#9192=EDGE_CURVE('',#7371,#7370,#4468,.T.);
#9193=EDGE_CURVE('',#7371,#7368,#4469,.T.);
#9194=EDGE_CURVE('',#7372,#7370,#4470,.T.);
#9195=EDGE_CURVE('',#7373,#7372,#4471,.T.);
#9196=EDGE_CURVE('',#7373,#7371,#4472,.T.);
#9197=EDGE_CURVE('',#7367,#7372,#4473,.T.);
#9198=EDGE_CURVE('',#7369,#7373,#4474,.T.);
#9199=EDGE_CURVE('',#7374,#7375,#4475,.T.);
#9200=EDGE_CURVE('',#7376,#7374,#4476,.T.);
#9201=EDGE_CURVE('',#7376,#7377,#4477,.T.);
#9202=EDGE_CURVE('',#7377,#7375,#4478,.T.);
#9203=EDGE_CURVE('',#7378,#7374,#4479,.T.);
#9204=EDGE_CURVE('',#7379,#7378,#4480,.T.);
#9205=EDGE_CURVE('',#7379,#7376,#4481,.T.);
#9206=EDGE_CURVE('',#7380,#7378,#4482,.T.);
#9207=EDGE_CURVE('',#7381,#7380,#4483,.T.);
#9208=EDGE_CURVE('',#7381,#7379,#4484,.T.);
#9209=EDGE_CURVE('',#7375,#7380,#4485,.T.);
#9210=EDGE_CURVE('',#7377,#7381,#4486,.T.);
#9211=EDGE_CURVE('',#7382,#7383,#4487,.T.);
#9212=EDGE_CURVE('',#7384,#7383,#4488,.T.);
#9213=EDGE_CURVE('',#7385,#7384,#4489,.T.);
#9214=EDGE_CURVE('',#7385,#7382,#4490,.T.);
#9215=EDGE_CURVE('',#7386,#7382,#4491,.T.);
#9216=EDGE_CURVE('',#7387,#7385,#4492,.T.);
#9217=EDGE_CURVE('',#7387,#7386,#4493,.T.);
#9218=EDGE_CURVE('',#7388,#7386,#4494,.T.);
#9219=EDGE_CURVE('',#7389,#7387,#4495,.T.);
#9220=EDGE_CURVE('',#7389,#7388,#4496,.T.);
#9221=EDGE_CURVE('',#7383,#7388,#4497,.T.);
#9222=EDGE_CURVE('',#7384,#7389,#4498,.T.);
#9223=EDGE_CURVE('',#7390,#7390,#1011,.T.);
#9224=EDGE_CURVE('',#7390,#7391,#4499,.T.);
#9225=EDGE_CURVE('',#7391,#7391,#1012,.T.);
#9226=EDGE_CURVE('',#7392,#7392,#1013,.T.);
#9227=EDGE_CURVE('',#7392,#7393,#4500,.T.);
#9228=EDGE_CURVE('',#7393,#7393,#1014,.T.);
#9229=EDGE_CURVE('',#7394,#7394,#1015,.T.);
#9230=EDGE_CURVE('',#7394,#7395,#4501,.T.);
#9231=EDGE_CURVE('',#7395,#7395,#1016,.T.);
#9232=EDGE_CURVE('',#7396,#7396,#1017,.T.);
#9233=EDGE_CURVE('',#7396,#7397,#4502,.T.);
#9234=EDGE_CURVE('',#7397,#7397,#1018,.T.);
#9235=EDGE_CURVE('',#7398,#7399,#4503,.T.);
#9236=EDGE_CURVE('',#7399,#7400,#4504,.T.);
#9237=EDGE_CURVE('',#7400,#7401,#4505,.T.);
#9238=EDGE_CURVE('',#7401,#7398,#4506,.T.);
#9239=EDGE_CURVE('',#7402,#7403,#4507,.T.);
#9240=EDGE_CURVE('',#7404,#7402,#4508,.T.);
#9241=EDGE_CURVE('',#7405,#7404,#4509,.T.);
#9242=EDGE_CURVE('',#7403,#7405,#4510,.T.);
#9243=EDGE_CURVE('',#7399,#7403,#4511,.T.);
#9244=EDGE_CURVE('',#7398,#7402,#4512,.T.);
#9245=EDGE_CURVE('',#7400,#7405,#4513,.T.);
#9246=EDGE_CURVE('',#7401,#7404,#4514,.T.);
#9247=EDGE_CURVE('',#7406,#7406,#1019,.T.);
#9248=EDGE_CURVE('',#7406,#7407,#4515,.T.);
#9249=EDGE_CURVE('',#7407,#7407,#1020,.T.);
#9250=EDGE_CURVE('',#7408,#7408,#1021,.T.);
#9251=EDGE_CURVE('',#7408,#7409,#4516,.T.);
#9252=EDGE_CURVE('',#7409,#7409,#1022,.T.);
#9253=EDGE_CURVE('',#7410,#7410,#1023,.T.);
#9254=EDGE_CURVE('',#7410,#7411,#4517,.T.);
#9255=EDGE_CURVE('',#7411,#7411,#1024,.T.);
#9256=EDGE_CURVE('',#7412,#7412,#1025,.T.);
#9257=EDGE_CURVE('',#7412,#7413,#4518,.T.);
#9258=EDGE_CURVE('',#7413,#7413,#1026,.T.);
#9259=EDGE_CURVE('',#7414,#7414,#1027,.T.);
#9260=EDGE_CURVE('',#7414,#7415,#4519,.T.);
#9261=EDGE_CURVE('',#7415,#7415,#1028,.T.);
#9262=EDGE_CURVE('',#7416,#7416,#1029,.T.);
#9263=EDGE_CURVE('',#7416,#7417,#4520,.T.);
#9264=EDGE_CURVE('',#7417,#7417,#1030,.T.);
#9265=EDGE_CURVE('',#7418,#7419,#4521,.T.);
#9266=EDGE_CURVE('',#7420,#7418,#4522,.T.);
#9267=EDGE_CURVE('',#7420,#7421,#4523,.T.);
#9268=EDGE_CURVE('',#7421,#7419,#4524,.T.);
#9269=EDGE_CURVE('',#7422,#7418,#4525,.T.);
#9270=EDGE_CURVE('',#7423,#7422,#4526,.T.);
#9271=EDGE_CURVE('',#7423,#7420,#4527,.T.);
#9272=EDGE_CURVE('',#7424,#7422,#4528,.T.);
#9273=EDGE_CURVE('',#7425,#7424,#4529,.T.);
#9274=EDGE_CURVE('',#7425,#7423,#4530,.T.);
#9275=EDGE_CURVE('',#7419,#7424,#4531,.T.);
#9276=EDGE_CURVE('',#7421,#7425,#4532,.T.);
#9277=EDGE_CURVE('',#7426,#7427,#4533,.T.);
#9278=EDGE_CURVE('',#7428,#7427,#4534,.T.);
#9279=EDGE_CURVE('',#7429,#7428,#4535,.T.);
#9280=EDGE_CURVE('',#7429,#7426,#4536,.T.);
#9281=EDGE_CURVE('',#7427,#7430,#4537,.T.);
#9282=EDGE_CURVE('',#7431,#7430,#4538,.T.);
#9283=EDGE_CURVE('',#7428,#7431,#4539,.T.);
#9284=EDGE_CURVE('',#7430,#7432,#4540,.T.);
#9285=EDGE_CURVE('',#7433,#7432,#4541,.T.);
#9286=EDGE_CURVE('',#7431,#7433,#4542,.T.);
#9287=EDGE_CURVE('',#7432,#7434,#4543,.T.);
#9288=EDGE_CURVE('',#7435,#7434,#4544,.T.);
#9289=EDGE_CURVE('',#7433,#7435,#4545,.T.);
#9290=EDGE_CURVE('',#7434,#7436,#4546,.T.);
#9291=EDGE_CURVE('',#7437,#7436,#4547,.T.);
#9292=EDGE_CURVE('',#7435,#7437,#4548,.T.);
#9293=EDGE_CURVE('',#7436,#7438,#4549,.T.);
#9294=EDGE_CURVE('',#7439,#7438,#4550,.T.);
#9295=EDGE_CURVE('',#7437,#7439,#4551,.T.);
#9296=EDGE_CURVE('',#7438,#7426,#4552,.T.);
#9297=EDGE_CURVE('',#7439,#7429,#4553,.T.);
#9298=EDGE_CURVE('',#7440,#7441,#4554,.T.);
#9299=EDGE_CURVE('',#7442,#7441,#4555,.T.);
#9300=EDGE_CURVE('',#7443,#7442,#4556,.T.);
#9301=EDGE_CURVE('',#7443,#7440,#4557,.T.);
#9302=EDGE_CURVE('',#7441,#7444,#4558,.T.);
#9303=EDGE_CURVE('',#7445,#7444,#4559,.T.);
#9304=EDGE_CURVE('',#7442,#7445,#4560,.T.);
#9305=EDGE_CURVE('',#7444,#7446,#4561,.T.);
#9306=EDGE_CURVE('',#7447,#7446,#4562,.T.);
#9307=EDGE_CURVE('',#7445,#7447,#4563,.T.);
#9308=EDGE_CURVE('',#7446,#7448,#4564,.T.);
#9309=EDGE_CURVE('',#7449,#7448,#4565,.T.);
#9310=EDGE_CURVE('',#7447,#7449,#4566,.T.);
#9311=EDGE_CURVE('',#7448,#7450,#4567,.T.);
#9312=EDGE_CURVE('',#7451,#7450,#4568,.T.);
#9313=EDGE_CURVE('',#7449,#7451,#4569,.T.);
#9314=EDGE_CURVE('',#7450,#7452,#4570,.T.);
#9315=EDGE_CURVE('',#7453,#7452,#4571,.T.);
#9316=EDGE_CURVE('',#7451,#7453,#4572,.T.);
#9317=EDGE_CURVE('',#7452,#7440,#4573,.T.);
#9318=EDGE_CURVE('',#7453,#7443,#4574,.T.);
#9319=EDGE_CURVE('',#7454,#7455,#4575,.T.);
#9320=EDGE_CURVE('',#7456,#7455,#4576,.T.);
#9321=EDGE_CURVE('',#7457,#7456,#4577,.T.);
#9322=EDGE_CURVE('',#7457,#7454,#4578,.T.);
#9323=EDGE_CURVE('',#7455,#7458,#4579,.T.);
#9324=EDGE_CURVE('',#7459,#7458,#4580,.T.);
#9325=EDGE_CURVE('',#7456,#7459,#4581,.T.);
#9326=EDGE_CURVE('',#7458,#7460,#4582,.T.);
#9327=EDGE_CURVE('',#7461,#7460,#4583,.T.);
#9328=EDGE_CURVE('',#7459,#7461,#4584,.T.);
#9329=EDGE_CURVE('',#7460,#7462,#4585,.T.);
#9330=EDGE_CURVE('',#7463,#7462,#4586,.T.);
#9331=EDGE_CURVE('',#7461,#7463,#4587,.T.);
#9332=EDGE_CURVE('',#7462,#7464,#4588,.T.);
#9333=EDGE_CURVE('',#7465,#7464,#4589,.T.);
#9334=EDGE_CURVE('',#7463,#7465,#4590,.T.);
#9335=EDGE_CURVE('',#7464,#7466,#4591,.T.);
#9336=EDGE_CURVE('',#7467,#7466,#4592,.T.);
#9337=EDGE_CURVE('',#7465,#7467,#4593,.T.);
#9338=EDGE_CURVE('',#7466,#7454,#4594,.T.);
#9339=EDGE_CURVE('',#7467,#7457,#4595,.T.);
#9340=EDGE_CURVE('',#7468,#7469,#4596,.T.);
#9341=EDGE_CURVE('',#7470,#7468,#4597,.T.);
#9342=EDGE_CURVE('',#7470,#7471,#4598,.T.);
#9343=EDGE_CURVE('',#7471,#7469,#4599,.T.);
#9344=EDGE_CURVE('',#7472,#7468,#4600,.T.);
#9345=EDGE_CURVE('',#7473,#7472,#4601,.T.);
#9346=EDGE_CURVE('',#7473,#7470,#4602,.T.);
#9347=EDGE_CURVE('',#7474,#7472,#4603,.T.);
#9348=EDGE_CURVE('',#7475,#7474,#4604,.T.);
#9349=EDGE_CURVE('',#7475,#7473,#4605,.T.);
#9350=EDGE_CURVE('',#7476,#7474,#4606,.T.);
#9351=EDGE_CURVE('',#7477,#7476,#4607,.T.);
#9352=EDGE_CURVE('',#7477,#7475,#4608,.T.);
#9353=EDGE_CURVE('',#7478,#7476,#4609,.T.);
#9354=EDGE_CURVE('',#7479,#7478,#4610,.T.);
#9355=EDGE_CURVE('',#7479,#7477,#4611,.T.);
#9356=EDGE_CURVE('',#7480,#7478,#4612,.T.);
#9357=EDGE_CURVE('',#7481,#7480,#4613,.T.);
#9358=EDGE_CURVE('',#7481,#7479,#4614,.T.);
#9359=EDGE_CURVE('',#7469,#7480,#4615,.T.);
#9360=EDGE_CURVE('',#7471,#7481,#4616,.T.);
#9361=EDGE_CURVE('',#7482,#7483,#4617,.T.);
#9362=EDGE_CURVE('',#7484,#7482,#4618,.T.);
#9363=EDGE_CURVE('',#7484,#7485,#4619,.T.);
#9364=EDGE_CURVE('',#7485,#7483,#4620,.T.);
#9365=EDGE_CURVE('',#7486,#7482,#4621,.T.);
#9366=EDGE_CURVE('',#7487,#7486,#4622,.T.);
#9367=EDGE_CURVE('',#7487,#7484,#4623,.T.);
#9368=EDGE_CURVE('',#7488,#7486,#4624,.T.);
#9369=EDGE_CURVE('',#7489,#7488,#4625,.T.);
#9370=EDGE_CURVE('',#7489,#7487,#4626,.T.);
#9371=EDGE_CURVE('',#7490,#7488,#4627,.T.);
#9372=EDGE_CURVE('',#7491,#7490,#4628,.T.);
#9373=EDGE_CURVE('',#7491,#7489,#4629,.T.);
#9374=EDGE_CURVE('',#7492,#7490,#4630,.T.);
#9375=EDGE_CURVE('',#7493,#7492,#4631,.T.);
#9376=EDGE_CURVE('',#7493,#7491,#4632,.T.);
#9377=EDGE_CURVE('',#7494,#7492,#4633,.T.);
#9378=EDGE_CURVE('',#7495,#7494,#4634,.T.);
#9379=EDGE_CURVE('',#7495,#7493,#4635,.T.);
#9380=EDGE_CURVE('',#7483,#7494,#4636,.T.);
#9381=EDGE_CURVE('',#7485,#7495,#4637,.T.);
#9382=EDGE_CURVE('',#7496,#7497,#4638,.T.);
#9383=EDGE_CURVE('',#7498,#7496,#4639,.T.);
#9384=EDGE_CURVE('',#7498,#7499,#4640,.T.);
#9385=EDGE_CURVE('',#7499,#7497,#4641,.T.);
#9386=EDGE_CURVE('',#7500,#7496,#4642,.T.);
#9387=EDGE_CURVE('',#7501,#7500,#4643,.T.);
#9388=EDGE_CURVE('',#7501,#7498,#4644,.T.);
#9389=EDGE_CURVE('',#7502,#7500,#4645,.T.);
#9390=EDGE_CURVE('',#7503,#7502,#4646,.T.);
#9391=EDGE_CURVE('',#7503,#7501,#4647,.T.);
#9392=EDGE_CURVE('',#7504,#7502,#4648,.T.);
#9393=EDGE_CURVE('',#7505,#7504,#4649,.T.);
#9394=EDGE_CURVE('',#7505,#7503,#4650,.T.);
#9395=EDGE_CURVE('',#7506,#7504,#4651,.T.);
#9396=EDGE_CURVE('',#7507,#7506,#4652,.T.);
#9397=EDGE_CURVE('',#7507,#7505,#4653,.T.);
#9398=EDGE_CURVE('',#7508,#7506,#4654,.T.);
#9399=EDGE_CURVE('',#7509,#7508,#4655,.T.);
#9400=EDGE_CURVE('',#7509,#7507,#4656,.T.);
#9401=EDGE_CURVE('',#7497,#7508,#4657,.T.);
#9402=EDGE_CURVE('',#7499,#7509,#4658,.T.);
#9403=EDGE_CURVE('',#7510,#7511,#4659,.T.);
#9404=EDGE_CURVE('',#7512,#7511,#4660,.T.);
#9405=EDGE_CURVE('',#7513,#7512,#4661,.T.);
#9406=EDGE_CURVE('',#7513,#7510,#4662,.T.);
#9407=EDGE_CURVE('',#7514,#7510,#4663,.T.);
#9408=EDGE_CURVE('',#7515,#7513,#4664,.T.);
#9409=EDGE_CURVE('',#7515,#7514,#4665,.T.);
#9410=EDGE_CURVE('',#7516,#7514,#4666,.T.);
#9411=EDGE_CURVE('',#7517,#7515,#4667,.T.);
#9412=EDGE_CURVE('',#7517,#7516,#4668,.T.);
#9413=EDGE_CURVE('',#7518,#7516,#4669,.T.);
#9414=EDGE_CURVE('',#7519,#7517,#4670,.T.);
#9415=EDGE_CURVE('',#7519,#7518,#4671,.T.);
#9416=EDGE_CURVE('',#7520,#7518,#4672,.T.);
#9417=EDGE_CURVE('',#7521,#7519,#4673,.T.);
#9418=EDGE_CURVE('',#7521,#7520,#4674,.T.);
#9419=EDGE_CURVE('',#7522,#7520,#4675,.T.);
#9420=EDGE_CURVE('',#7523,#7521,#4676,.T.);
#9421=EDGE_CURVE('',#7523,#7522,#4677,.T.);
#9422=EDGE_CURVE('',#7511,#7522,#4678,.T.);
#9423=EDGE_CURVE('',#7512,#7523,#4679,.T.);
#9424=EDGE_CURVE('',#7524,#7525,#4680,.T.);
#9425=EDGE_CURVE('',#7526,#7525,#4681,.T.);
#9426=EDGE_CURVE('',#7527,#7526,#4682,.T.);
#9427=EDGE_CURVE('',#7527,#7524,#4683,.T.);
#9428=EDGE_CURVE('',#7528,#7524,#4684,.T.);
#9429=EDGE_CURVE('',#7529,#7527,#4685,.T.);
#9430=EDGE_CURVE('',#7529,#7528,#4686,.T.);
#9431=EDGE_CURVE('',#7530,#7528,#4687,.T.);
#9432=EDGE_CURVE('',#7531,#7529,#4688,.T.);
#9433=EDGE_CURVE('',#7531,#7530,#4689,.T.);
#9434=EDGE_CURVE('',#7532,#7530,#4690,.T.);
#9435=EDGE_CURVE('',#7533,#7531,#4691,.T.);
#9436=EDGE_CURVE('',#7533,#7532,#4692,.T.);
#9437=EDGE_CURVE('',#7534,#7532,#4693,.T.);
#9438=EDGE_CURVE('',#7535,#7533,#4694,.T.);
#9439=EDGE_CURVE('',#7535,#7534,#4695,.T.);
#9440=EDGE_CURVE('',#7536,#7534,#4696,.T.);
#9441=EDGE_CURVE('',#7537,#7535,#4697,.T.);
#9442=EDGE_CURVE('',#7537,#7536,#4698,.T.);
#9443=EDGE_CURVE('',#7525,#7536,#4699,.T.);
#9444=EDGE_CURVE('',#7526,#7537,#4700,.T.);
#9445=EDGE_CURVE('',#7538,#7539,#4701,.T.);
#9446=EDGE_CURVE('',#7540,#7538,#4702,.T.);
#9447=EDGE_CURVE('',#7540,#7541,#4703,.T.);
#9448=EDGE_CURVE('',#7541,#7539,#4704,.T.);
#9449=EDGE_CURVE('',#7539,#7542,#4705,.T.);
#9450=EDGE_CURVE('',#7541,#7543,#4706,.T.);
#9451=EDGE_CURVE('',#7543,#7542,#4707,.T.);
#9452=EDGE_CURVE('',#7542,#7544,#4708,.T.);
#9453=EDGE_CURVE('',#7543,#7545,#4709,.T.);
#9454=EDGE_CURVE('',#7545,#7544,#4710,.T.);
#9455=EDGE_CURVE('',#7544,#7546,#4711,.T.);
#9456=EDGE_CURVE('',#7545,#7547,#4712,.T.);
#9457=EDGE_CURVE('',#7547,#7546,#4713,.T.);
#9458=EDGE_CURVE('',#7546,#7548,#4714,.T.);
#9459=EDGE_CURVE('',#7547,#7549,#4715,.T.);
#9460=EDGE_CURVE('',#7549,#7548,#4716,.T.);
#9461=EDGE_CURVE('',#7548,#7550,#4717,.T.);
#9462=EDGE_CURVE('',#7549,#7551,#4718,.T.);
#9463=EDGE_CURVE('',#7551,#7550,#4719,.T.);
#9464=EDGE_CURVE('',#7550,#7538,#4720,.T.);
#9465=EDGE_CURVE('',#7551,#7540,#4721,.T.);
#9466=EDGE_CURVE('',#7552,#7553,#4722,.T.);
#9467=EDGE_CURVE('',#7554,#7552,#4723,.T.);
#9468=EDGE_CURVE('',#7554,#7555,#4724,.T.);
#9469=EDGE_CURVE('',#7555,#7553,#4725,.T.);
#9470=EDGE_CURVE('',#7553,#7556,#4726,.T.);
#9471=EDGE_CURVE('',#7555,#7557,#4727,.T.);
#9472=EDGE_CURVE('',#7557,#7556,#4728,.T.);
#9473=EDGE_CURVE('',#7556,#7558,#4729,.T.);
#9474=EDGE_CURVE('',#7557,#7559,#4730,.T.);
#9475=EDGE_CURVE('',#7559,#7558,#4731,.T.);
#9476=EDGE_CURVE('',#7558,#7560,#4732,.T.);
#9477=EDGE_CURVE('',#7559,#7561,#4733,.T.);
#9478=EDGE_CURVE('',#7561,#7560,#4734,.T.);
#9479=EDGE_CURVE('',#7560,#7562,#4735,.T.);
#9480=EDGE_CURVE('',#7561,#7563,#4736,.T.);
#9481=EDGE_CURVE('',#7563,#7562,#4737,.T.);
#9482=EDGE_CURVE('',#7562,#7564,#4738,.T.);
#9483=EDGE_CURVE('',#7563,#7565,#4739,.T.);
#9484=EDGE_CURVE('',#7565,#7564,#4740,.T.);
#9485=EDGE_CURVE('',#7564,#7552,#4741,.T.);
#9486=EDGE_CURVE('',#7565,#7554,#4742,.T.);
#9487=EDGE_CURVE('',#7566,#7567,#4743,.T.);
#9488=EDGE_CURVE('',#7568,#7566,#4744,.T.);
#9489=EDGE_CURVE('',#7568,#7569,#4745,.T.);
#9490=EDGE_CURVE('',#7569,#7567,#4746,.T.);
#9491=EDGE_CURVE('',#7567,#7570,#4747,.T.);
#9492=EDGE_CURVE('',#7569,#7571,#4748,.T.);
#9493=EDGE_CURVE('',#7571,#7570,#4749,.T.);
#9494=EDGE_CURVE('',#7570,#7572,#4750,.T.);
#9495=EDGE_CURVE('',#7571,#7573,#4751,.T.);
#9496=EDGE_CURVE('',#7573,#7572,#4752,.T.);
#9497=EDGE_CURVE('',#7572,#7574,#4753,.T.);
#9498=EDGE_CURVE('',#7573,#7575,#4754,.T.);
#9499=EDGE_CURVE('',#7575,#7574,#4755,.T.);
#9500=EDGE_CURVE('',#7574,#7576,#4756,.T.);
#9501=EDGE_CURVE('',#7575,#7577,#4757,.T.);
#9502=EDGE_CURVE('',#7577,#7576,#4758,.T.);
#9503=EDGE_CURVE('',#7576,#7578,#4759,.T.);
#9504=EDGE_CURVE('',#7577,#7579,#4760,.T.);
#9505=EDGE_CURVE('',#7579,#7578,#4761,.T.);
#9506=EDGE_CURVE('',#7578,#7566,#4762,.T.);
#9507=EDGE_CURVE('',#7579,#7568,#4763,.T.);
#9508=EDGE_CURVE('',#7580,#7580,#1031,.T.);
#9509=EDGE_CURVE('',#7580,#7581,#4764,.T.);
#9510=EDGE_CURVE('',#7581,#7581,#1032,.T.);
#9511=EDGE_CURVE('',#7582,#7582,#1033,.T.);
#9512=EDGE_CURVE('',#7582,#7583,#4765,.T.);
#9513=EDGE_CURVE('',#7583,#7583,#1034,.T.);
#9514=EDGE_CURVE('',#7584,#7584,#1035,.T.);
#9515=EDGE_CURVE('',#7584,#7585,#4766,.T.);
#9516=EDGE_CURVE('',#7585,#7585,#1036,.T.);
#9517=EDGE_CURVE('',#7586,#7586,#1037,.T.);
#9518=EDGE_CURVE('',#7586,#7587,#4767,.T.);
#9519=EDGE_CURVE('',#7587,#7587,#1038,.T.);
#9520=EDGE_CURVE('',#7588,#7589,#4768,.T.);
#9521=EDGE_CURVE('',#7590,#7588,#4769,.T.);
#9522=EDGE_CURVE('',#7591,#7590,#4770,.T.);
#9523=EDGE_CURVE('',#7589,#7591,#4771,.T.);
#9524=EDGE_CURVE('',#7592,#7593,#4772,.T.);
#9525=EDGE_CURVE('',#7593,#7594,#4773,.T.);
#9526=EDGE_CURVE('',#7594,#7595,#4774,.T.);
#9527=EDGE_CURVE('',#7595,#7592,#4775,.T.);
#9528=EDGE_CURVE('',#7588,#7592,#4776,.T.);
#9529=EDGE_CURVE('',#7589,#7593,#4777,.T.);
#9530=EDGE_CURVE('',#7591,#7594,#4778,.T.);
#9531=EDGE_CURVE('',#7590,#7595,#4779,.T.);
#9532=EDGE_CURVE('',#7596,#7597,#4780,.T.);
#9533=EDGE_CURVE('',#7598,#7597,#4781,.T.);
#9534=EDGE_CURVE('',#7599,#7598,#4782,.T.);
#9535=EDGE_CURVE('',#7599,#7596,#4783,.T.);
#9536=EDGE_CURVE('',#7597,#7600,#4784,.T.);
#9537=EDGE_CURVE('',#7601,#7600,#4785,.T.);
#9538=EDGE_CURVE('',#7598,#7601,#4786,.T.);
#9539=EDGE_CURVE('',#7600,#7602,#4787,.T.);
#9540=EDGE_CURVE('',#7603,#7602,#4788,.T.);
#9541=EDGE_CURVE('',#7601,#7603,#4789,.T.);
#9542=EDGE_CURVE('',#7602,#7596,#4790,.T.);
#9543=EDGE_CURVE('',#7603,#7599,#4791,.T.);
#9544=EDGE_CURVE('',#7604,#7605,#4792,.T.);
#9545=EDGE_CURVE('',#7606,#7605,#4793,.T.);
#9546=EDGE_CURVE('',#7607,#7606,#4794,.T.);
#9547=EDGE_CURVE('',#7607,#7604,#4795,.T.);
#9548=EDGE_CURVE('',#7605,#7608,#4796,.T.);
#9549=EDGE_CURVE('',#7609,#7608,#4797,.T.);
#9550=EDGE_CURVE('',#7606,#7609,#4798,.T.);
#9551=EDGE_CURVE('',#7608,#7610,#4799,.T.);
#9552=EDGE_CURVE('',#7611,#7610,#4800,.T.);
#9553=EDGE_CURVE('',#7609,#7611,#4801,.T.);
#9554=EDGE_CURVE('',#7610,#7604,#4802,.T.);
#9555=EDGE_CURVE('',#7611,#7607,#4803,.T.);
#9556=EDGE_CURVE('',#7612,#7613,#4804,.T.);
#9557=EDGE_CURVE('',#7614,#7613,#4805,.T.);
#9558=EDGE_CURVE('',#7615,#7614,#4806,.T.);
#9559=EDGE_CURVE('',#7615,#7612,#4807,.T.);
#9560=EDGE_CURVE('',#7613,#7616,#4808,.T.);
#9561=EDGE_CURVE('',#7617,#7616,#4809,.T.);
#9562=EDGE_CURVE('',#7614,#7617,#4810,.T.);
#9563=EDGE_CURVE('',#7616,#7618,#4811,.T.);
#9564=EDGE_CURVE('',#7619,#7618,#4812,.T.);
#9565=EDGE_CURVE('',#7617,#7619,#4813,.T.);
#9566=EDGE_CURVE('',#7618,#7612,#4814,.T.);
#9567=EDGE_CURVE('',#7619,#7615,#4815,.T.);
#9568=EDGE_CURVE('',#7620,#7621,#4816,.T.);
#9569=EDGE_CURVE('',#7622,#7621,#4817,.T.);
#9570=EDGE_CURVE('',#7623,#7622,#4818,.T.);
#9571=EDGE_CURVE('',#7623,#7620,#4819,.T.);
#9572=EDGE_CURVE('',#7621,#7624,#4820,.T.);
#9573=EDGE_CURVE('',#7625,#7624,#4821,.T.);
#9574=EDGE_CURVE('',#7622,#7625,#4822,.T.);
#9575=EDGE_CURVE('',#7624,#7626,#4823,.T.);
#9576=EDGE_CURVE('',#7627,#7626,#4824,.T.);
#9577=EDGE_CURVE('',#7625,#7627,#4825,.T.);
#9578=EDGE_CURVE('',#7626,#7620,#4826,.T.);
#9579=EDGE_CURVE('',#7627,#7623,#4827,.T.);
#9580=EDGE_CURVE('',#7628,#7629,#4828,.T.);
#9581=EDGE_CURVE('',#7630,#7629,#4829,.T.);
#9582=EDGE_CURVE('',#7631,#7630,#4830,.T.);
#9583=EDGE_CURVE('',#7631,#7628,#4831,.T.);
#9584=EDGE_CURVE('',#7629,#7632,#4832,.T.);
#9585=EDGE_CURVE('',#7633,#7632,#4833,.T.);
#9586=EDGE_CURVE('',#7630,#7633,#4834,.T.);
#9587=EDGE_CURVE('',#7632,#7634,#4835,.T.);
#9588=EDGE_CURVE('',#7635,#7634,#4836,.T.);
#9589=EDGE_CURVE('',#7633,#7635,#4837,.T.);
#9590=EDGE_CURVE('',#7634,#7628,#4838,.T.);
#9591=EDGE_CURVE('',#7635,#7631,#4839,.T.);
#9592=EDGE_CURVE('',#7636,#7637,#4840,.T.);
#9593=EDGE_CURVE('',#7638,#7637,#4841,.T.);
#9594=EDGE_CURVE('',#7639,#7638,#4842,.T.);
#9595=EDGE_CURVE('',#7639,#7636,#4843,.T.);
#9596=EDGE_CURVE('',#7637,#7640,#4844,.T.);
#9597=EDGE_CURVE('',#7641,#7640,#4845,.T.);
#9598=EDGE_CURVE('',#7638,#7641,#4846,.T.);
#9599=EDGE_CURVE('',#7640,#7642,#4847,.T.);
#9600=EDGE_CURVE('',#7643,#7642,#4848,.T.);
#9601=EDGE_CURVE('',#7641,#7643,#4849,.T.);
#9602=EDGE_CURVE('',#7642,#7636,#4850,.T.);
#9603=EDGE_CURVE('',#7643,#7639,#4851,.T.);
#9604=EDGE_CURVE('',#7644,#7645,#4852,.T.);
#9605=EDGE_CURVE('',#7646,#7645,#4853,.T.);
#9606=EDGE_CURVE('',#7647,#7646,#4854,.T.);
#9607=EDGE_CURVE('',#7647,#7644,#4855,.T.);
#9608=EDGE_CURVE('',#7645,#7648,#4856,.T.);
#9609=EDGE_CURVE('',#7649,#7648,#4857,.T.);
#9610=EDGE_CURVE('',#7646,#7649,#4858,.T.);
#9611=EDGE_CURVE('',#7648,#7650,#4859,.T.);
#9612=EDGE_CURVE('',#7651,#7650,#4860,.T.);
#9613=EDGE_CURVE('',#7649,#7651,#4861,.T.);
#9614=EDGE_CURVE('',#7650,#7644,#4862,.T.);
#9615=EDGE_CURVE('',#7651,#7647,#4863,.T.);
#9616=EDGE_CURVE('',#7652,#7653,#4864,.T.);
#9617=EDGE_CURVE('',#7654,#7653,#4865,.T.);
#9618=EDGE_CURVE('',#7655,#7654,#4866,.T.);
#9619=EDGE_CURVE('',#7655,#7652,#4867,.T.);
#9620=EDGE_CURVE('',#7653,#7656,#4868,.T.);
#9621=EDGE_CURVE('',#7657,#7656,#4869,.T.);
#9622=EDGE_CURVE('',#7654,#7657,#4870,.T.);
#9623=EDGE_CURVE('',#7656,#7658,#4871,.T.);
#9624=EDGE_CURVE('',#7659,#7658,#4872,.T.);
#9625=EDGE_CURVE('',#7657,#7659,#4873,.T.);
#9626=EDGE_CURVE('',#7658,#7652,#4874,.T.);
#9627=EDGE_CURVE('',#7659,#7655,#4875,.T.);
#9628=EDGE_CURVE('',#7660,#7661,#4876,.T.);
#9629=EDGE_CURVE('',#7662,#7661,#4877,.T.);
#9630=EDGE_CURVE('',#7663,#7662,#4878,.T.);
#9631=EDGE_CURVE('',#7663,#7660,#4879,.T.);
#9632=EDGE_CURVE('',#7661,#7664,#4880,.T.);
#9633=EDGE_CURVE('',#7665,#7664,#4881,.T.);
#9634=EDGE_CURVE('',#7662,#7665,#4882,.T.);
#9635=EDGE_CURVE('',#7664,#7666,#4883,.T.);
#9636=EDGE_CURVE('',#7667,#7666,#4884,.T.);
#9637=EDGE_CURVE('',#7665,#7667,#4885,.T.);
#9638=EDGE_CURVE('',#7666,#7660,#4886,.T.);
#9639=EDGE_CURVE('',#7667,#7663,#4887,.T.);
#9640=EDGE_CURVE('',#7668,#7669,#4888,.T.);
#9641=EDGE_CURVE('',#7670,#7669,#4889,.T.);
#9642=EDGE_CURVE('',#7671,#7670,#4890,.T.);
#9643=EDGE_CURVE('',#7671,#7668,#4891,.T.);
#9644=EDGE_CURVE('',#7669,#7672,#4892,.T.);
#9645=EDGE_CURVE('',#7673,#7672,#4893,.T.);
#9646=EDGE_CURVE('',#7670,#7673,#4894,.T.);
#9647=EDGE_CURVE('',#7672,#7674,#4895,.T.);
#9648=EDGE_CURVE('',#7675,#7674,#4896,.T.);
#9649=EDGE_CURVE('',#7673,#7675,#4897,.T.);
#9650=EDGE_CURVE('',#7674,#7668,#4898,.T.);
#9651=EDGE_CURVE('',#7675,#7671,#4899,.T.);
#9652=EDGE_CURVE('',#7676,#7677,#4900,.T.);
#9653=EDGE_CURVE('',#7678,#7677,#4901,.T.);
#9654=EDGE_CURVE('',#7679,#7678,#4902,.T.);
#9655=EDGE_CURVE('',#7679,#7676,#4903,.T.);
#9656=EDGE_CURVE('',#7677,#7680,#4904,.T.);
#9657=EDGE_CURVE('',#7681,#7680,#4905,.T.);
#9658=EDGE_CURVE('',#7678,#7681,#4906,.T.);
#9659=EDGE_CURVE('',#7680,#7682,#4907,.T.);
#9660=EDGE_CURVE('',#7683,#7682,#4908,.T.);
#9661=EDGE_CURVE('',#7681,#7683,#4909,.T.);
#9662=EDGE_CURVE('',#7682,#7676,#4910,.T.);
#9663=EDGE_CURVE('',#7683,#7679,#4911,.T.);
#9664=EDGE_CURVE('',#7684,#7685,#4912,.T.);
#9665=EDGE_CURVE('',#7686,#7684,#4913,.T.);
#9666=EDGE_CURVE('',#7686,#7687,#4914,.T.);
#9667=EDGE_CURVE('',#7687,#7685,#4915,.T.);
#9668=EDGE_CURVE('',#7685,#7688,#4916,.T.);
#9669=EDGE_CURVE('',#7687,#7689,#4917,.T.);
#9670=EDGE_CURVE('',#7689,#7688,#4918,.T.);
#9671=EDGE_CURVE('',#7688,#7690,#4919,.T.);
#9672=EDGE_CURVE('',#7689,#7691,#4920,.T.);
#9673=EDGE_CURVE('',#7691,#7690,#4921,.T.);
#9674=EDGE_CURVE('',#7690,#7684,#4922,.T.);
#9675=EDGE_CURVE('',#7691,#7686,#4923,.T.);
#9676=EDGE_CURVE('',#7692,#7693,#4924,.T.);
#9677=EDGE_CURVE('',#7694,#7692,#4925,.T.);
#9678=EDGE_CURVE('',#7694,#7695,#4926,.T.);
#9679=EDGE_CURVE('',#7695,#7693,#4927,.T.);
#9680=EDGE_CURVE('',#7693,#7696,#4928,.T.);
#9681=EDGE_CURVE('',#7695,#7697,#4929,.T.);
#9682=EDGE_CURVE('',#7697,#7696,#4930,.T.);
#9683=EDGE_CURVE('',#7696,#7698,#4931,.T.);
#9684=EDGE_CURVE('',#7697,#7699,#4932,.T.);
#9685=EDGE_CURVE('',#7699,#7698,#4933,.T.);
#9686=EDGE_CURVE('',#7698,#7692,#4934,.T.);
#9687=EDGE_CURVE('',#7699,#7694,#4935,.T.);
#9688=EDGE_CURVE('',#7700,#7701,#4936,.T.);
#9689=EDGE_CURVE('',#7702,#7700,#4937,.T.);
#9690=EDGE_CURVE('',#7702,#7703,#4938,.T.);
#9691=EDGE_CURVE('',#7703,#7701,#4939,.T.);
#9692=EDGE_CURVE('',#7701,#7704,#4940,.T.);
#9693=EDGE_CURVE('',#7703,#7705,#4941,.T.);
#9694=EDGE_CURVE('',#7705,#7704,#4942,.T.);
#9695=EDGE_CURVE('',#7704,#7706,#4943,.T.);
#9696=EDGE_CURVE('',#7705,#7707,#4944,.T.);
#9697=EDGE_CURVE('',#7707,#7706,#4945,.T.);
#9698=EDGE_CURVE('',#7706,#7700,#4946,.T.);
#9699=EDGE_CURVE('',#7707,#7702,#4947,.T.);
#9700=EDGE_CURVE('',#7708,#7709,#4948,.T.);
#9701=EDGE_CURVE('',#7710,#7708,#4949,.T.);
#9702=EDGE_CURVE('',#7710,#7711,#4950,.T.);
#9703=EDGE_CURVE('',#7711,#7709,#4951,.T.);
#9704=EDGE_CURVE('',#7709,#7712,#4952,.T.);
#9705=EDGE_CURVE('',#7711,#7713,#4953,.T.);
#9706=EDGE_CURVE('',#7713,#7712,#4954,.T.);
#9707=EDGE_CURVE('',#7712,#7714,#4955,.T.);
#9708=EDGE_CURVE('',#7713,#7715,#4956,.T.);
#9709=EDGE_CURVE('',#7715,#7714,#4957,.T.);
#9710=EDGE_CURVE('',#7714,#7708,#4958,.T.);
#9711=EDGE_CURVE('',#7715,#7710,#4959,.T.);
#9712=EDGE_CURVE('',#7716,#7717,#4960,.T.);
#9713=EDGE_CURVE('',#7718,#7716,#4961,.T.);
#9714=EDGE_CURVE('',#7718,#7719,#4962,.T.);
#9715=EDGE_CURVE('',#7719,#7717,#4963,.T.);
#9716=EDGE_CURVE('',#7717,#7720,#4964,.T.);
#9717=EDGE_CURVE('',#7719,#7721,#4965,.T.);
#9718=EDGE_CURVE('',#7721,#7720,#4966,.T.);
#9719=EDGE_CURVE('',#7720,#7722,#4967,.T.);
#9720=EDGE_CURVE('',#7721,#7723,#4968,.T.);
#9721=EDGE_CURVE('',#7723,#7722,#4969,.T.);
#9722=EDGE_CURVE('',#7722,#7716,#4970,.T.);
#9723=EDGE_CURVE('',#7723,#7718,#4971,.T.);
#9724=EDGE_CURVE('',#7724,#7725,#4972,.T.);
#9725=EDGE_CURVE('',#7726,#7725,#4973,.T.);
#9726=EDGE_CURVE('',#7727,#7726,#4974,.T.);
#9727=EDGE_CURVE('',#7727,#7724,#4975,.T.);
#9728=EDGE_CURVE('',#7725,#7728,#4976,.T.);
#9729=EDGE_CURVE('',#7729,#7728,#4977,.T.);
#9730=EDGE_CURVE('',#7726,#7729,#4978,.T.);
#9731=EDGE_CURVE('',#7728,#7730,#4979,.T.);
#9732=EDGE_CURVE('',#7731,#7730,#4980,.T.);
#9733=EDGE_CURVE('',#7729,#7731,#4981,.T.);
#9734=EDGE_CURVE('',#7730,#7724,#4982,.T.);
#9735=EDGE_CURVE('',#7731,#7727,#4983,.T.);
#9736=EDGE_CURVE('',#7732,#7733,#4984,.T.);
#9737=EDGE_CURVE('',#7734,#7733,#4985,.T.);
#9738=EDGE_CURVE('',#7735,#7734,#4986,.T.);
#9739=EDGE_CURVE('',#7735,#7732,#4987,.T.);
#9740=EDGE_CURVE('',#7733,#7736,#4988,.T.);
#9741=EDGE_CURVE('',#7737,#7736,#4989,.T.);
#9742=EDGE_CURVE('',#7734,#7737,#4990,.T.);
#9743=EDGE_CURVE('',#7736,#7738,#4991,.T.);
#9744=EDGE_CURVE('',#7739,#7738,#4992,.T.);
#9745=EDGE_CURVE('',#7737,#7739,#4993,.T.);
#9746=EDGE_CURVE('',#7738,#7732,#4994,.T.);
#9747=EDGE_CURVE('',#7739,#7735,#4995,.T.);
#9748=EDGE_CURVE('',#7740,#7741,#4996,.T.);
#9749=EDGE_CURVE('',#7742,#7741,#4997,.T.);
#9750=EDGE_CURVE('',#7743,#7742,#4998,.T.);
#9751=EDGE_CURVE('',#7743,#7740,#4999,.T.);
#9752=EDGE_CURVE('',#7741,#7744,#5000,.T.);
#9753=EDGE_CURVE('',#7745,#7744,#5001,.T.);
#9754=EDGE_CURVE('',#7742,#7745,#5002,.T.);
#9755=EDGE_CURVE('',#7744,#7746,#5003,.T.);
#9756=EDGE_CURVE('',#7747,#7746,#5004,.T.);
#9757=EDGE_CURVE('',#7745,#7747,#5005,.T.);
#9758=EDGE_CURVE('',#7746,#7740,#5006,.T.);
#9759=EDGE_CURVE('',#7747,#7743,#5007,.T.);
#9760=EDGE_CURVE('',#7748,#7749,#5008,.T.);
#9761=EDGE_CURVE('',#7750,#7749,#5009,.T.);
#9762=EDGE_CURVE('',#7751,#7750,#5010,.T.);
#9763=EDGE_CURVE('',#7751,#7748,#5011,.T.);
#9764=EDGE_CURVE('',#7749,#7752,#5012,.T.);
#9765=EDGE_CURVE('',#7753,#7752,#5013,.T.);
#9766=EDGE_CURVE('',#7750,#7753,#5014,.T.);
#9767=EDGE_CURVE('',#7752,#7754,#5015,.T.);
#9768=EDGE_CURVE('',#7755,#7754,#5016,.T.);
#9769=EDGE_CURVE('',#7753,#7755,#5017,.T.);
#9770=EDGE_CURVE('',#7754,#7748,#5018,.T.);
#9771=EDGE_CURVE('',#7755,#7751,#5019,.T.);
#9772=EDGE_CURVE('',#7756,#7757,#5020,.T.);
#9773=EDGE_CURVE('',#7758,#7757,#5021,.T.);
#9774=EDGE_CURVE('',#7759,#7758,#5022,.T.);
#9775=EDGE_CURVE('',#7759,#7756,#5023,.T.);
#9776=EDGE_CURVE('',#7757,#7760,#5024,.T.);
#9777=EDGE_CURVE('',#7761,#7760,#5025,.T.);
#9778=EDGE_CURVE('',#7758,#7761,#5026,.T.);
#9779=EDGE_CURVE('',#7760,#7762,#5027,.T.);
#9780=EDGE_CURVE('',#7763,#7762,#5028,.T.);
#9781=EDGE_CURVE('',#7761,#7763,#5029,.T.);
#9782=EDGE_CURVE('',#7762,#7756,#5030,.T.);
#9783=EDGE_CURVE('',#7763,#7759,#5031,.T.);
#9784=EDGE_CURVE('',#7764,#7765,#5032,.T.);
#9785=EDGE_CURVE('',#7766,#7765,#5033,.T.);
#9786=EDGE_CURVE('',#7767,#7766,#5034,.T.);
#9787=EDGE_CURVE('',#7767,#7764,#5035,.T.);
#9788=EDGE_CURVE('',#7765,#7768,#5036,.T.);
#9789=EDGE_CURVE('',#7769,#7768,#5037,.T.);
#9790=EDGE_CURVE('',#7766,#7769,#5038,.T.);
#9791=EDGE_CURVE('',#7768,#7770,#5039,.T.);
#9792=EDGE_CURVE('',#7771,#7770,#5040,.T.);
#9793=EDGE_CURVE('',#7769,#7771,#5041,.T.);
#9794=EDGE_CURVE('',#7770,#7764,#5042,.T.);
#9795=EDGE_CURVE('',#7771,#7767,#5043,.T.);
#9796=EDGE_CURVE('',#7772,#7773,#1039,.T.);
#9797=EDGE_CURVE('',#7773,#7772,#1040,.T.);
#9798=EDGE_CURVE('',#7773,#7774,#1041,.T.);
#9799=EDGE_CURVE('',#7774,#7774,#1042,.T.);
#9800=EDGE_CURVE('',#7775,#7776,#1043,.T.);
#9801=EDGE_CURVE('',#7777,#7775,#1044,.T.);
#9802=EDGE_CURVE('',#7778,#7777,#1045,.T.);
#9803=EDGE_CURVE('',#7778,#7779,#5044,.T.);
#9804=EDGE_CURVE('',#7779,#7779,#1046,.T.);
#9805=EDGE_CURVE('',#7780,#7778,#1047,.T.);
#9806=EDGE_CURVE('',#7781,#7780,#1048,.T.);
#9807=EDGE_CURVE('',#7776,#7781,#1049,.T.);
#9808=EDGE_CURVE('',#7782,#7782,#1050,.T.);
#9809=EDGE_CURVE('',#7782,#7783,#5045,.T.);
#9810=EDGE_CURVE('',#7783,#7783,#1051,.T.);
#9811=EDGE_CURVE('',#7772,#7782,#5046,.T.);
#9812=EDGE_CURVE('',#7784,#7780,#5047,.T.);
#9813=EDGE_CURVE('',#7778,#7784,#5048,.T.);
#9814=EDGE_CURVE('',#7780,#7785,#5049,.T.);
#9815=EDGE_CURVE('',#7785,#7781,#5050,.T.);
#9816=EDGE_CURVE('',#7781,#7786,#5051,.T.);
#9817=EDGE_CURVE('',#7786,#7776,#5052,.T.);
#9818=EDGE_CURVE('',#7776,#7787,#5053,.T.);
#9819=EDGE_CURVE('',#7787,#7775,#5054,.T.);
#9820=EDGE_CURVE('',#7775,#7788,#5055,.T.);
#9821=EDGE_CURVE('',#7788,#7777,#5056,.T.);
#9822=EDGE_CURVE('',#7777,#7789,#5057,.T.);
#9823=EDGE_CURVE('',#7789,#7778,#5058,.T.);
#9824=EDGE_CURVE('',#7790,#7791,#1052,.T.);
#9825=EDGE_CURVE('',#7792,#7790,#1053,.T.);
#9826=EDGE_CURVE('',#7793,#7792,#1054,.T.);
#9827=EDGE_CURVE('',#7794,#7793,#1055,.T.);
#9828=EDGE_CURVE('',#7794,#7795,#1056,.T.);
#9829=EDGE_CURVE('',#7791,#7795,#1057,.T.);
#9830=EDGE_CURVE('',#7795,#7796,#538,.T.);
#9831=EDGE_CURVE('',#7796,#7791,#539,.T.);
#9832=EDGE_CURVE('',#7794,#7797,#540,.T.);
#9833=EDGE_CURVE('',#7797,#7795,#541,.T.);
#9834=EDGE_CURVE('',#7798,#7794,#542,.T.);
#9835=EDGE_CURVE('',#7793,#7798,#543,.T.);
#9836=EDGE_CURVE('',#7799,#7793,#544,.T.);
#9837=EDGE_CURVE('',#7792,#7799,#545,.T.);
#9838=EDGE_CURVE('',#7791,#7800,#546,.T.);
#9839=EDGE_CURVE('',#7800,#7790,#547,.T.);
#9840=EDGE_CURVE('',#7801,#7792,#548,.T.);
#9841=EDGE_CURVE('',#7790,#7801,#549,.T.);
#9842=EDGE_CURVE('',#7789,#7801,#5059,.T.);
#9843=EDGE_CURVE('',#7784,#7800,#5060,.T.);
#9844=EDGE_CURVE('',#7788,#7799,#5061,.T.);
#9845=EDGE_CURVE('',#7787,#7798,#5062,.T.);
#9846=EDGE_CURVE('',#7786,#7797,#5063,.T.);
#9847=EDGE_CURVE('',#7785,#7796,#5064,.T.);
#9848=EDGE_CURVE('',#7802,#7802,#1058,.T.);
#9849=EDGE_CURVE('',#7802,#7803,#5065,.T.);
#9850=EDGE_CURVE('',#7803,#7803,#1059,.T.);
#9851=EDGE_CURVE('',#7804,#7804,#1060,.T.);
#9852=EDGE_CURVE('',#7804,#7805,#5066,.T.);
#9853=EDGE_CURVE('',#7805,#7805,#1061,.T.);
#9854=EDGE_CURVE('',#7806,#7806,#1062,.T.);
#9855=EDGE_CURVE('',#7806,#7807,#5067,.T.);
#9856=EDGE_CURVE('',#7807,#7808,#1063,.T.);
#9857=EDGE_CURVE('',#7808,#7807,#1064,.T.);
#9858=EDGE_CURVE('',#7809,#7810,#1065,.T.);
#9859=EDGE_CURVE('',#7810,#7808,#5068,.T.);
#9860=EDGE_CURVE('',#7810,#7809,#1066,.T.);
#9861=EDGE_CURVE('',#7811,#7811,#1067,.T.);
#9862=EDGE_CURVE('',#7811,#7812,#5069,.T.);
#9863=EDGE_CURVE('',#7812,#7812,#1068,.T.);
#9864=EDGE_CURVE('',#7809,#7811,#5070,.T.);
#9865=EDGE_CURVE('',#7813,#7814,#5071,.T.);
#9866=EDGE_CURVE('',#7814,#7815,#550,.T.);
#9867=EDGE_CURVE('',#7815,#7816,#551,.T.);
#9868=EDGE_CURVE('',#7817,#7816,#5072,.T.);
#9869=EDGE_CURVE('',#7818,#7817,#552,.T.);
#9870=EDGE_CURVE('',#7813,#7818,#553,.T.);
#9871=EDGE_CURVE('',#7816,#7819,#554,.T.);
#9872=EDGE_CURVE('',#7819,#7820,#555,.T.);
#9873=EDGE_CURVE('',#7821,#7820,#5073,.T.);
#9874=EDGE_CURVE('',#7822,#7821,#556,.T.);
#9875=EDGE_CURVE('',#7817,#7822,#557,.T.);
#9876=EDGE_CURVE('',#7823,#7824,#558,.T.);
#9877=EDGE_CURVE('',#7825,#7823,#5074,.T.);
#9878=EDGE_CURVE('',#7825,#7826,#559,.T.);
#9879=EDGE_CURVE('',#7826,#7821,#560,.T.);
#9880=EDGE_CURVE('',#7824,#7820,#561,.T.);
#9881=EDGE_CURVE('',#7823,#7827,#562,.T.);
#9882=EDGE_CURVE('',#7827,#7828,#563,.T.);
#9883=EDGE_CURVE('',#7829,#7828,#5075,.T.);
#9884=EDGE_CURVE('',#7830,#7829,#564,.T.);
#9885=EDGE_CURVE('',#7825,#7830,#565,.T.);
#9886=EDGE_CURVE('',#7828,#7831,#566,.T.);
#9887=EDGE_CURVE('',#7831,#7832,#567,.T.);
#9888=EDGE_CURVE('',#7833,#7832,#5076,.T.);
#9889=EDGE_CURVE('',#7834,#7833,#568,.T.);
#9890=EDGE_CURVE('',#7829,#7834,#569,.T.);
#9891=EDGE_CURVE('',#7832,#7835,#570,.T.);
#9892=EDGE_CURVE('',#7835,#7814,#571,.T.);
#9893=EDGE_CURVE('',#7836,#7813,#572,.T.);
#9894=EDGE_CURVE('',#7833,#7836,#573,.T.);
#9895=EDGE_CURVE('',#7835,#7815,#1069,.T.);
#9896=EDGE_CURVE('',#7831,#7835,#1070,.T.);
#9897=EDGE_CURVE('',#7827,#7831,#1071,.T.);
#9898=EDGE_CURVE('',#7824,#7827,#1072,.T.);
#9899=EDGE_CURVE('',#7824,#7819,#1073,.T.);
#9900=EDGE_CURVE('',#7815,#7819,#1074,.T.);
#9901=EDGE_CURVE('',#7836,#7834,#1075,.T.);
#9902=EDGE_CURVE('',#7818,#7836,#1076,.T.);
#9903=EDGE_CURVE('',#7822,#7818,#1077,.T.);
#9904=EDGE_CURVE('',#7826,#7822,#1078,.T.);
#9905=EDGE_CURVE('',#7830,#7826,#1079,.T.);
#9906=EDGE_CURVE('',#7834,#7830,#1080,.T.);
#9907=ORIENTED_EDGE('',*,*,#7837,.F.);
#9908=ORIENTED_EDGE('',*,*,#7838,.F.);
#9909=ORIENTED_EDGE('',*,*,#7839,.T.);
#9910=ORIENTED_EDGE('',*,*,#7840,.T.);
#9911=ORIENTED_EDGE('',*,*,#7841,.F.);
#9912=ORIENTED_EDGE('',*,*,#7842,.F.);
#9913=ORIENTED_EDGE('',*,*,#7843,.T.);
#9914=ORIENTED_EDGE('',*,*,#7838,.T.);
#9915=ORIENTED_EDGE('',*,*,#7844,.F.);
#9916=ORIENTED_EDGE('',*,*,#7845,.F.);
#9917=ORIENTED_EDGE('',*,*,#7846,.T.);
#9918=ORIENTED_EDGE('',*,*,#7842,.T.);
#9919=ORIENTED_EDGE('',*,*,#7847,.F.);
#9920=ORIENTED_EDGE('',*,*,#7840,.F.);
#9921=ORIENTED_EDGE('',*,*,#7848,.T.);
#9922=ORIENTED_EDGE('',*,*,#7845,.T.);
#9923=ORIENTED_EDGE('',*,*,#7839,.F.);
#9924=ORIENTED_EDGE('',*,*,#7843,.F.);
#9925=ORIENTED_EDGE('',*,*,#7846,.F.);
#9926=ORIENTED_EDGE('',*,*,#7848,.F.);
#9927=ORIENTED_EDGE('',*,*,#7849,.T.);
#9928=ORIENTED_EDGE('',*,*,#7850,.T.);
#9929=ORIENTED_EDGE('',*,*,#7851,.T.);
#9930=ORIENTED_EDGE('',*,*,#7852,.T.);
#9931=ORIENTED_EDGE('',*,*,#7837,.T.);
#9932=ORIENTED_EDGE('',*,*,#7847,.T.);
#9933=ORIENTED_EDGE('',*,*,#7844,.T.);
#9934=ORIENTED_EDGE('',*,*,#7841,.T.);
#9935=ORIENTED_EDGE('',*,*,#7853,.F.);
#9936=ORIENTED_EDGE('',*,*,#7854,.F.);
#9937=ORIENTED_EDGE('',*,*,#7855,.F.);
#9938=ORIENTED_EDGE('',*,*,#7856,.F.);
#9939=ORIENTED_EDGE('',*,*,#7854,.T.);
#9940=ORIENTED_EDGE('',*,*,#7857,.F.);
#9941=ORIENTED_EDGE('',*,*,#7849,.F.);
#9942=ORIENTED_EDGE('',*,*,#7858,.T.);
#9943=ORIENTED_EDGE('',*,*,#7855,.T.);
#9944=ORIENTED_EDGE('',*,*,#7858,.F.);
#9945=ORIENTED_EDGE('',*,*,#7852,.F.);
#9946=ORIENTED_EDGE('',*,*,#7859,.T.);
#9947=ORIENTED_EDGE('',*,*,#7856,.T.);
#9948=ORIENTED_EDGE('',*,*,#7859,.F.);
#9949=ORIENTED_EDGE('',*,*,#7851,.F.);
#9950=ORIENTED_EDGE('',*,*,#7860,.T.);
#9951=ORIENTED_EDGE('',*,*,#7853,.T.);
#9952=ORIENTED_EDGE('',*,*,#7860,.F.);
#9953=ORIENTED_EDGE('',*,*,#7850,.F.);
#9954=ORIENTED_EDGE('',*,*,#7857,.T.);
#9955=ORIENTED_EDGE('',*,*,#7861,.T.);
#9956=ORIENTED_EDGE('',*,*,#7862,.F.);
#9957=ORIENTED_EDGE('',*,*,#7863,.F.);
#9958=ORIENTED_EDGE('',*,*,#7864,.T.);
#9959=ORIENTED_EDGE('',*,*,#7865,.T.);
#9960=ORIENTED_EDGE('',*,*,#7866,.F.);
#9961=ORIENTED_EDGE('',*,*,#7867,.F.);
#9962=ORIENTED_EDGE('',*,*,#7862,.T.);
#9963=ORIENTED_EDGE('',*,*,#7868,.T.);
#9964=ORIENTED_EDGE('',*,*,#7869,.F.);
#9965=ORIENTED_EDGE('',*,*,#7870,.F.);
#9966=ORIENTED_EDGE('',*,*,#7866,.T.);
#9967=ORIENTED_EDGE('',*,*,#7871,.T.);
#9968=ORIENTED_EDGE('',*,*,#7872,.F.);
#9969=ORIENTED_EDGE('',*,*,#7873,.F.);
#9970=ORIENTED_EDGE('',*,*,#7869,.T.);
#9971=ORIENTED_EDGE('',*,*,#7874,.T.);
#9972=ORIENTED_EDGE('',*,*,#7875,.F.);
#9973=ORIENTED_EDGE('',*,*,#7876,.F.);
#9974=ORIENTED_EDGE('',*,*,#7872,.T.);
#9975=ORIENTED_EDGE('',*,*,#7877,.T.);
#9976=ORIENTED_EDGE('',*,*,#7864,.F.);
#9977=ORIENTED_EDGE('',*,*,#7878,.F.);
#9978=ORIENTED_EDGE('',*,*,#7875,.T.);
#9979=ORIENTED_EDGE('',*,*,#7863,.T.);
#9980=ORIENTED_EDGE('',*,*,#7867,.T.);
#9981=ORIENTED_EDGE('',*,*,#7870,.T.);
#9982=ORIENTED_EDGE('',*,*,#7873,.T.);
#9983=ORIENTED_EDGE('',*,*,#7876,.T.);
#9984=ORIENTED_EDGE('',*,*,#7878,.T.);
#9985=ORIENTED_EDGE('',*,*,#7861,.F.);
#9986=ORIENTED_EDGE('',*,*,#7877,.F.);
#9987=ORIENTED_EDGE('',*,*,#7874,.F.);
#9988=ORIENTED_EDGE('',*,*,#7871,.F.);
#9989=ORIENTED_EDGE('',*,*,#7868,.F.);
#9990=ORIENTED_EDGE('',*,*,#7865,.F.);
#9991=ORIENTED_EDGE('',*,*,#7879,.F.);
#9992=ORIENTED_EDGE('',*,*,#7880,.F.);
#9993=ORIENTED_EDGE('',*,*,#7881,.T.);
#9994=ORIENTED_EDGE('',*,*,#7882,.T.);
#9995=ORIENTED_EDGE('',*,*,#7883,.F.);
#9996=ORIENTED_EDGE('',*,*,#7882,.F.);
#9997=ORIENTED_EDGE('',*,*,#7884,.T.);
#9998=ORIENTED_EDGE('',*,*,#7885,.T.);
#9999=ORIENTED_EDGE('',*,*,#7886,.F.);
#10000=ORIENTED_EDGE('',*,*,#7885,.F.);
#10001=ORIENTED_EDGE('',*,*,#7887,.T.);
#10002=ORIENTED_EDGE('',*,*,#7888,.T.);
#10003=ORIENTED_EDGE('',*,*,#7889,.F.);
#10004=ORIENTED_EDGE('',*,*,#7888,.F.);
#10005=ORIENTED_EDGE('',*,*,#7890,.T.);
#10006=ORIENTED_EDGE('',*,*,#7891,.T.);
#10007=ORIENTED_EDGE('',*,*,#7892,.F.);
#10008=ORIENTED_EDGE('',*,*,#7891,.F.);
#10009=ORIENTED_EDGE('',*,*,#7893,.T.);
#10010=ORIENTED_EDGE('',*,*,#7894,.T.);
#10011=ORIENTED_EDGE('',*,*,#7895,.F.);
#10012=ORIENTED_EDGE('',*,*,#7894,.F.);
#10013=ORIENTED_EDGE('',*,*,#7896,.T.);
#10014=ORIENTED_EDGE('',*,*,#7880,.T.);
#10015=ORIENTED_EDGE('',*,*,#7881,.F.);
#10016=ORIENTED_EDGE('',*,*,#7896,.F.);
#10017=ORIENTED_EDGE('',*,*,#7893,.F.);
#10018=ORIENTED_EDGE('',*,*,#7890,.F.);
#10019=ORIENTED_EDGE('',*,*,#7887,.F.);
#10020=ORIENTED_EDGE('',*,*,#7884,.F.);
#10021=ORIENTED_EDGE('',*,*,#7879,.T.);
#10022=ORIENTED_EDGE('',*,*,#7883,.T.);
#10023=ORIENTED_EDGE('',*,*,#7886,.T.);
#10024=ORIENTED_EDGE('',*,*,#7889,.T.);
#10025=ORIENTED_EDGE('',*,*,#7892,.T.);
#10026=ORIENTED_EDGE('',*,*,#7895,.T.);
#10027=ORIENTED_EDGE('',*,*,#7897,.T.);
#10028=ORIENTED_EDGE('',*,*,#7898,.T.);
#10029=ORIENTED_EDGE('',*,*,#7899,.F.);
#10030=ORIENTED_EDGE('',*,*,#7898,.F.);
#10031=ORIENTED_EDGE('',*,*,#7900,.T.);
#10032=ORIENTED_EDGE('',*,*,#7901,.T.);
#10033=ORIENTED_EDGE('',*,*,#7902,.F.);
#10034=ORIENTED_EDGE('',*,*,#7901,.F.);
#10035=ORIENTED_EDGE('',*,*,#7903,.T.);
#10036=ORIENTED_EDGE('',*,*,#7904,.T.);
#10037=ORIENTED_EDGE('',*,*,#7905,.F.);
#10038=ORIENTED_EDGE('',*,*,#7904,.F.);
#10039=ORIENTED_EDGE('',*,*,#7906,.T.);
#10040=ORIENTED_EDGE('',*,*,#7907,.T.);
#10041=ORIENTED_EDGE('',*,*,#7908,.F.);
#10042=ORIENTED_EDGE('',*,*,#7907,.F.);
#10043=ORIENTED_EDGE('',*,*,#7909,.T.);
#10044=ORIENTED_EDGE('',*,*,#7910,.T.);
#10045=ORIENTED_EDGE('',*,*,#7911,.F.);
#10046=ORIENTED_EDGE('',*,*,#7910,.F.);
#10047=ORIENTED_EDGE('',*,*,#7912,.T.);
#10048=ORIENTED_EDGE('',*,*,#7913,.T.);
#10049=ORIENTED_EDGE('',*,*,#7914,.F.);
#10050=ORIENTED_EDGE('',*,*,#7913,.F.);
#10051=ORIENTED_EDGE('',*,*,#7915,.T.);
#10052=ORIENTED_EDGE('',*,*,#7916,.T.);
#10053=ORIENTED_EDGE('',*,*,#7917,.T.);
#10054=ORIENTED_EDGE('',*,*,#7918,.T.);
#10055=ORIENTED_EDGE('',*,*,#7909,.F.);
#10056=ORIENTED_EDGE('',*,*,#7903,.F.);
#10057=ORIENTED_EDGE('',*,*,#7897,.F.);
#10058=ORIENTED_EDGE('',*,*,#7900,.F.);
#10059=ORIENTED_EDGE('',*,*,#7906,.F.);
#10060=ORIENTED_EDGE('',*,*,#7912,.F.);
#10061=ORIENTED_EDGE('',*,*,#7919,.F.);
#10062=ORIENTED_EDGE('',*,*,#7920,.F.);
#10063=ORIENTED_EDGE('',*,*,#7921,.F.);
#10064=ORIENTED_EDGE('',*,*,#7922,.F.);
#10065=ORIENTED_EDGE('',*,*,#7914,.T.);
#10066=ORIENTED_EDGE('',*,*,#7911,.T.);
#10067=ORIENTED_EDGE('',*,*,#7908,.T.);
#10068=ORIENTED_EDGE('',*,*,#7905,.T.);
#10069=ORIENTED_EDGE('',*,*,#7902,.T.);
#10070=ORIENTED_EDGE('',*,*,#7899,.T.);
#10071=ORIENTED_EDGE('',*,*,#7919,.T.);
#10072=ORIENTED_EDGE('',*,*,#7923,.F.);
#10073=ORIENTED_EDGE('',*,*,#7915,.F.);
#10074=ORIENTED_EDGE('',*,*,#7924,.T.);
#10075=ORIENTED_EDGE('',*,*,#7922,.T.);
#10076=ORIENTED_EDGE('',*,*,#7925,.F.);
#10077=ORIENTED_EDGE('',*,*,#7916,.F.);
#10078=ORIENTED_EDGE('',*,*,#7923,.T.);
#10079=ORIENTED_EDGE('',*,*,#7921,.T.);
#10080=ORIENTED_EDGE('',*,*,#7926,.F.);
#10081=ORIENTED_EDGE('',*,*,#7917,.F.);
#10082=ORIENTED_EDGE('',*,*,#7925,.T.);
#10083=ORIENTED_EDGE('',*,*,#7920,.T.);
#10084=ORIENTED_EDGE('',*,*,#7924,.F.);
#10085=ORIENTED_EDGE('',*,*,#7918,.F.);
#10086=ORIENTED_EDGE('',*,*,#7926,.T.);
#10087=ORIENTED_EDGE('',*,*,#7927,.F.);
#10088=ORIENTED_EDGE('',*,*,#7928,.T.);
#10089=ORIENTED_EDGE('',*,*,#7929,.T.);
#10090=ORIENTED_EDGE('',*,*,#7928,.F.);
#10091=ORIENTED_EDGE('',*,*,#7930,.F.);
#10092=ORIENTED_EDGE('',*,*,#7931,.T.);
#10093=ORIENTED_EDGE('',*,*,#7932,.T.);
#10094=ORIENTED_EDGE('',*,*,#7931,.F.);
#10095=ORIENTED_EDGE('',*,*,#7933,.F.);
#10096=ORIENTED_EDGE('',*,*,#7934,.T.);
#10097=ORIENTED_EDGE('',*,*,#7935,.T.);
#10098=ORIENTED_EDGE('',*,*,#7934,.F.);
#10099=ORIENTED_EDGE('',*,*,#7936,.F.);
#10100=ORIENTED_EDGE('',*,*,#7937,.T.);
#10101=ORIENTED_EDGE('',*,*,#7938,.T.);
#10102=ORIENTED_EDGE('',*,*,#7937,.F.);
#10103=ORIENTED_EDGE('',*,*,#7939,.F.);
#10104=ORIENTED_EDGE('',*,*,#7940,.T.);
#10105=ORIENTED_EDGE('',*,*,#7941,.T.);
#10106=ORIENTED_EDGE('',*,*,#7940,.F.);
#10107=ORIENTED_EDGE('',*,*,#7942,.F.);
#10108=ORIENTED_EDGE('',*,*,#7943,.F.);
#10109=ORIENTED_EDGE('',*,*,#7944,.T.);
#10110=ORIENTED_EDGE('',*,*,#7945,.T.);
#10111=ORIENTED_EDGE('',*,*,#7946,.F.);
#10112=ORIENTED_EDGE('',*,*,#7947,.F.);
#10113=ORIENTED_EDGE('',*,*,#7948,.T.);
#10114=ORIENTED_EDGE('',*,*,#7943,.T.);
#10115=ORIENTED_EDGE('',*,*,#7949,.F.);
#10116=ORIENTED_EDGE('',*,*,#7950,.F.);
#10117=ORIENTED_EDGE('',*,*,#7951,.T.);
#10118=ORIENTED_EDGE('',*,*,#7947,.T.);
#10119=ORIENTED_EDGE('',*,*,#7952,.F.);
#10120=ORIENTED_EDGE('',*,*,#7945,.F.);
#10121=ORIENTED_EDGE('',*,*,#7953,.T.);
#10122=ORIENTED_EDGE('',*,*,#7950,.T.);
#10123=ORIENTED_EDGE('',*,*,#7944,.F.);
#10124=ORIENTED_EDGE('',*,*,#7948,.F.);
#10125=ORIENTED_EDGE('',*,*,#7951,.F.);
#10126=ORIENTED_EDGE('',*,*,#7953,.F.);
#10127=ORIENTED_EDGE('',*,*,#7927,.T.);
#10128=ORIENTED_EDGE('',*,*,#7930,.T.);
#10129=ORIENTED_EDGE('',*,*,#7933,.T.);
#10130=ORIENTED_EDGE('',*,*,#7936,.T.);
#10131=ORIENTED_EDGE('',*,*,#7939,.T.);
#10132=ORIENTED_EDGE('',*,*,#7942,.T.);
#10133=ORIENTED_EDGE('',*,*,#7952,.T.);
#10134=ORIENTED_EDGE('',*,*,#7949,.T.);
#10135=ORIENTED_EDGE('',*,*,#7946,.T.);
#10136=ORIENTED_EDGE('',*,*,#7929,.F.);
#10137=ORIENTED_EDGE('',*,*,#7932,.F.);
#10138=ORIENTED_EDGE('',*,*,#7935,.F.);
#10139=ORIENTED_EDGE('',*,*,#7938,.F.);
#10140=ORIENTED_EDGE('',*,*,#7941,.F.);
#10141=ORIENTED_EDGE('',*,*,#7954,.T.);
#10142=ORIENTED_EDGE('',*,*,#7955,.T.);
#10143=ORIENTED_EDGE('',*,*,#7956,.F.);
#10144=ORIENTED_EDGE('',*,*,#7955,.F.);
#10145=ORIENTED_EDGE('',*,*,#7957,.T.);
#10146=ORIENTED_EDGE('',*,*,#7958,.T.);
#10147=ORIENTED_EDGE('',*,*,#7959,.F.);
#10148=ORIENTED_EDGE('',*,*,#7958,.F.);
#10149=ORIENTED_EDGE('',*,*,#7960,.T.);
#10150=ORIENTED_EDGE('',*,*,#7961,.T.);
#10151=ORIENTED_EDGE('',*,*,#7962,.F.);
#10152=ORIENTED_EDGE('',*,*,#7961,.F.);
#10153=ORIENTED_EDGE('',*,*,#7963,.T.);
#10154=ORIENTED_EDGE('',*,*,#7964,.T.);
#10155=ORIENTED_EDGE('',*,*,#7965,.F.);
#10156=ORIENTED_EDGE('',*,*,#7964,.F.);
#10157=ORIENTED_EDGE('',*,*,#7966,.T.);
#10158=ORIENTED_EDGE('',*,*,#7967,.T.);
#10159=ORIENTED_EDGE('',*,*,#7968,.F.);
#10160=ORIENTED_EDGE('',*,*,#7967,.F.);
#10161=ORIENTED_EDGE('',*,*,#7969,.T.);
#10162=ORIENTED_EDGE('',*,*,#7970,.F.);
#10163=ORIENTED_EDGE('',*,*,#7971,.F.);
#10164=ORIENTED_EDGE('',*,*,#7972,.T.);
#10165=ORIENTED_EDGE('',*,*,#7973,.T.);
#10166=ORIENTED_EDGE('',*,*,#7972,.F.);
#10167=ORIENTED_EDGE('',*,*,#7974,.F.);
#10168=ORIENTED_EDGE('',*,*,#7975,.T.);
#10169=ORIENTED_EDGE('',*,*,#7976,.T.);
#10170=ORIENTED_EDGE('',*,*,#7975,.F.);
#10171=ORIENTED_EDGE('',*,*,#7977,.F.);
#10172=ORIENTED_EDGE('',*,*,#7978,.T.);
#10173=ORIENTED_EDGE('',*,*,#7979,.T.);
#10174=ORIENTED_EDGE('',*,*,#7978,.F.);
#10175=ORIENTED_EDGE('',*,*,#7980,.F.);
#10176=ORIENTED_EDGE('',*,*,#7970,.T.);
#10177=ORIENTED_EDGE('',*,*,#7971,.T.);
#10178=ORIENTED_EDGE('',*,*,#7980,.T.);
#10179=ORIENTED_EDGE('',*,*,#7977,.T.);
#10180=ORIENTED_EDGE('',*,*,#7974,.T.);
#10181=ORIENTED_EDGE('',*,*,#7954,.F.);
#10182=ORIENTED_EDGE('',*,*,#7957,.F.);
#10183=ORIENTED_EDGE('',*,*,#7960,.F.);
#10184=ORIENTED_EDGE('',*,*,#7963,.F.);
#10185=ORIENTED_EDGE('',*,*,#7966,.F.);
#10186=ORIENTED_EDGE('',*,*,#7969,.F.);
#10187=ORIENTED_EDGE('',*,*,#7973,.F.);
#10188=ORIENTED_EDGE('',*,*,#7976,.F.);
#10189=ORIENTED_EDGE('',*,*,#7979,.F.);
#10190=ORIENTED_EDGE('',*,*,#7956,.T.);
#10191=ORIENTED_EDGE('',*,*,#7959,.T.);
#10192=ORIENTED_EDGE('',*,*,#7962,.T.);
#10193=ORIENTED_EDGE('',*,*,#7965,.T.);
#10194=ORIENTED_EDGE('',*,*,#7968,.T.);
#10195=ORIENTED_EDGE('',*,*,#7981,.T.);
#10196=ORIENTED_EDGE('',*,*,#7982,.F.);
#10197=ORIENTED_EDGE('',*,*,#7983,.F.);
#10198=ORIENTED_EDGE('',*,*,#7984,.T.);
#10199=ORIENTED_EDGE('',*,*,#7985,.T.);
#10200=ORIENTED_EDGE('',*,*,#7986,.F.);
#10201=ORIENTED_EDGE('',*,*,#7987,.F.);
#10202=ORIENTED_EDGE('',*,*,#7982,.T.);
#10203=ORIENTED_EDGE('',*,*,#7988,.T.);
#10204=ORIENTED_EDGE('',*,*,#7989,.F.);
#10205=ORIENTED_EDGE('',*,*,#7990,.F.);
#10206=ORIENTED_EDGE('',*,*,#7986,.T.);
#10207=ORIENTED_EDGE('',*,*,#7991,.T.);
#10208=ORIENTED_EDGE('',*,*,#7984,.F.);
#10209=ORIENTED_EDGE('',*,*,#7992,.F.);
#10210=ORIENTED_EDGE('',*,*,#7989,.T.);
#10211=ORIENTED_EDGE('',*,*,#7983,.T.);
#10212=ORIENTED_EDGE('',*,*,#7987,.T.);
#10213=ORIENTED_EDGE('',*,*,#7990,.T.);
#10214=ORIENTED_EDGE('',*,*,#7992,.T.);
#10215=ORIENTED_EDGE('',*,*,#7981,.F.);
#10216=ORIENTED_EDGE('',*,*,#7991,.F.);
#10217=ORIENTED_EDGE('',*,*,#7988,.F.);
#10218=ORIENTED_EDGE('',*,*,#7985,.F.);
#10219=ORIENTED_EDGE('',*,*,#7993,.T.);
#10220=ORIENTED_EDGE('',*,*,#7994,.F.);
#10221=ORIENTED_EDGE('',*,*,#7995,.F.);
#10222=ORIENTED_EDGE('',*,*,#7996,.T.);
#10223=ORIENTED_EDGE('',*,*,#7997,.T.);
#10224=ORIENTED_EDGE('',*,*,#7998,.F.);
#10225=ORIENTED_EDGE('',*,*,#7999,.F.);
#10226=ORIENTED_EDGE('',*,*,#7994,.T.);
#10227=ORIENTED_EDGE('',*,*,#8000,.T.);
#10228=ORIENTED_EDGE('',*,*,#8001,.F.);
#10229=ORIENTED_EDGE('',*,*,#8002,.F.);
#10230=ORIENTED_EDGE('',*,*,#7998,.T.);
#10231=ORIENTED_EDGE('',*,*,#8003,.T.);
#10232=ORIENTED_EDGE('',*,*,#7996,.F.);
#10233=ORIENTED_EDGE('',*,*,#8004,.F.);
#10234=ORIENTED_EDGE('',*,*,#8001,.T.);
#10235=ORIENTED_EDGE('',*,*,#7995,.T.);
#10236=ORIENTED_EDGE('',*,*,#7999,.T.);
#10237=ORIENTED_EDGE('',*,*,#8002,.T.);
#10238=ORIENTED_EDGE('',*,*,#8004,.T.);
#10239=ORIENTED_EDGE('',*,*,#7993,.F.);
#10240=ORIENTED_EDGE('',*,*,#8003,.F.);
#10241=ORIENTED_EDGE('',*,*,#8000,.F.);
#10242=ORIENTED_EDGE('',*,*,#7997,.F.);
#10243=ORIENTED_EDGE('',*,*,#8005,.F.);
#10244=ORIENTED_EDGE('',*,*,#8006,.F.);
#10245=ORIENTED_EDGE('',*,*,#8007,.T.);
#10246=ORIENTED_EDGE('',*,*,#8008,.T.);
#10247=ORIENTED_EDGE('',*,*,#8009,.F.);
#10248=ORIENTED_EDGE('',*,*,#8008,.F.);
#10249=ORIENTED_EDGE('',*,*,#8010,.T.);
#10250=ORIENTED_EDGE('',*,*,#8011,.T.);
#10251=ORIENTED_EDGE('',*,*,#8012,.F.);
#10252=ORIENTED_EDGE('',*,*,#8011,.F.);
#10253=ORIENTED_EDGE('',*,*,#8013,.T.);
#10254=ORIENTED_EDGE('',*,*,#8014,.T.);
#10255=ORIENTED_EDGE('',*,*,#8015,.F.);
#10256=ORIENTED_EDGE('',*,*,#8014,.F.);
#10257=ORIENTED_EDGE('',*,*,#8016,.T.);
#10258=ORIENTED_EDGE('',*,*,#8006,.T.);
#10259=ORIENTED_EDGE('',*,*,#8007,.F.);
#10260=ORIENTED_EDGE('',*,*,#8016,.F.);
#10261=ORIENTED_EDGE('',*,*,#8013,.F.);
#10262=ORIENTED_EDGE('',*,*,#8010,.F.);
#10263=ORIENTED_EDGE('',*,*,#8005,.T.);
#10264=ORIENTED_EDGE('',*,*,#8009,.T.);
#10265=ORIENTED_EDGE('',*,*,#8012,.T.);
#10266=ORIENTED_EDGE('',*,*,#8015,.T.);
#10267=ORIENTED_EDGE('',*,*,#8017,.F.);
#10268=ORIENTED_EDGE('',*,*,#8018,.T.);
#10269=ORIENTED_EDGE('',*,*,#8019,.T.);
#10270=ORIENTED_EDGE('',*,*,#8018,.F.);
#10271=ORIENTED_EDGE('',*,*,#8020,.F.);
#10272=ORIENTED_EDGE('',*,*,#8021,.T.);
#10273=ORIENTED_EDGE('',*,*,#8022,.T.);
#10274=ORIENTED_EDGE('',*,*,#8021,.F.);
#10275=ORIENTED_EDGE('',*,*,#8023,.F.);
#10276=ORIENTED_EDGE('',*,*,#8024,.T.);
#10277=ORIENTED_EDGE('',*,*,#8025,.T.);
#10278=ORIENTED_EDGE('',*,*,#8024,.F.);
#10279=ORIENTED_EDGE('',*,*,#8026,.F.);
#10280=ORIENTED_EDGE('',*,*,#8027,.T.);
#10281=ORIENTED_EDGE('',*,*,#8028,.T.);
#10282=ORIENTED_EDGE('',*,*,#8027,.F.);
#10283=ORIENTED_EDGE('',*,*,#8029,.F.);
#10284=ORIENTED_EDGE('',*,*,#8030,.T.);
#10285=ORIENTED_EDGE('',*,*,#8031,.T.);
#10286=ORIENTED_EDGE('',*,*,#8030,.F.);
#10287=ORIENTED_EDGE('',*,*,#8032,.F.);
#10288=ORIENTED_EDGE('',*,*,#8033,.T.);
#10289=ORIENTED_EDGE('',*,*,#8034,.T.);
#10290=ORIENTED_EDGE('',*,*,#8033,.F.);
#10291=ORIENTED_EDGE('',*,*,#8035,.F.);
#10292=ORIENTED_EDGE('',*,*,#8036,.T.);
#10293=ORIENTED_EDGE('',*,*,#8037,.T.);
#10294=ORIENTED_EDGE('',*,*,#8036,.F.);
#10295=ORIENTED_EDGE('',*,*,#8038,.F.);
#10296=ORIENTED_EDGE('',*,*,#8039,.T.);
#10297=ORIENTED_EDGE('',*,*,#8040,.T.);
#10298=ORIENTED_EDGE('',*,*,#8039,.F.);
#10299=ORIENTED_EDGE('',*,*,#8041,.F.);
#10300=ORIENTED_EDGE('',*,*,#8042,.T.);
#10301=ORIENTED_EDGE('',*,*,#8043,.T.);
#10302=ORIENTED_EDGE('',*,*,#8042,.F.);
#10303=ORIENTED_EDGE('',*,*,#8044,.F.);
#10304=ORIENTED_EDGE('',*,*,#8045,.T.);
#10305=ORIENTED_EDGE('',*,*,#8046,.T.);
#10306=ORIENTED_EDGE('',*,*,#8045,.F.);
#10307=ORIENTED_EDGE('',*,*,#8047,.F.);
#10308=ORIENTED_EDGE('',*,*,#8048,.T.);
#10309=ORIENTED_EDGE('',*,*,#8049,.T.);
#10310=ORIENTED_EDGE('',*,*,#8048,.F.);
#10311=ORIENTED_EDGE('',*,*,#8050,.F.);
#10312=ORIENTED_EDGE('',*,*,#8051,.T.);
#10313=ORIENTED_EDGE('',*,*,#8052,.T.);
#10314=ORIENTED_EDGE('',*,*,#8051,.F.);
#10315=ORIENTED_EDGE('',*,*,#8053,.F.);
#10316=ORIENTED_EDGE('',*,*,#8054,.T.);
#10317=ORIENTED_EDGE('',*,*,#8055,.T.);
#10318=ORIENTED_EDGE('',*,*,#8054,.F.);
#10319=ORIENTED_EDGE('',*,*,#8056,.F.);
#10320=ORIENTED_EDGE('',*,*,#8057,.T.);
#10321=ORIENTED_EDGE('',*,*,#8058,.T.);
#10322=ORIENTED_EDGE('',*,*,#8057,.F.);
#10323=ORIENTED_EDGE('',*,*,#8059,.F.);
#10324=ORIENTED_EDGE('',*,*,#8060,.T.);
#10325=ORIENTED_EDGE('',*,*,#8061,.T.);
#10326=ORIENTED_EDGE('',*,*,#8060,.F.);
#10327=ORIENTED_EDGE('',*,*,#8062,.F.);
#10328=ORIENTED_EDGE('',*,*,#8063,.T.);
#10329=ORIENTED_EDGE('',*,*,#8064,.T.);
#10330=ORIENTED_EDGE('',*,*,#8063,.F.);
#10331=ORIENTED_EDGE('',*,*,#8065,.F.);
#10332=ORIENTED_EDGE('',*,*,#8066,.T.);
#10333=ORIENTED_EDGE('',*,*,#8067,.T.);
#10334=ORIENTED_EDGE('',*,*,#8066,.F.);
#10335=ORIENTED_EDGE('',*,*,#8068,.F.);
#10336=ORIENTED_EDGE('',*,*,#8069,.T.);
#10337=ORIENTED_EDGE('',*,*,#8070,.T.);
#10338=ORIENTED_EDGE('',*,*,#8069,.F.);
#10339=ORIENTED_EDGE('',*,*,#8071,.F.);
#10340=ORIENTED_EDGE('',*,*,#8072,.F.);
#10341=ORIENTED_EDGE('',*,*,#8073,.T.);
#10342=ORIENTED_EDGE('',*,*,#8074,.T.);
#10343=ORIENTED_EDGE('',*,*,#8075,.F.);
#10344=ORIENTED_EDGE('',*,*,#8076,.F.);
#10345=ORIENTED_EDGE('',*,*,#8077,.T.);
#10346=ORIENTED_EDGE('',*,*,#8072,.T.);
#10347=ORIENTED_EDGE('',*,*,#8078,.F.);
#10348=ORIENTED_EDGE('',*,*,#8079,.F.);
#10349=ORIENTED_EDGE('',*,*,#8080,.T.);
#10350=ORIENTED_EDGE('',*,*,#8076,.T.);
#10351=ORIENTED_EDGE('',*,*,#8081,.F.);
#10352=ORIENTED_EDGE('',*,*,#8074,.F.);
#10353=ORIENTED_EDGE('',*,*,#8082,.T.);
#10354=ORIENTED_EDGE('',*,*,#8079,.T.);
#10355=ORIENTED_EDGE('',*,*,#8073,.F.);
#10356=ORIENTED_EDGE('',*,*,#8077,.F.);
#10357=ORIENTED_EDGE('',*,*,#8080,.F.);
#10358=ORIENTED_EDGE('',*,*,#8082,.F.);
#10359=ORIENTED_EDGE('',*,*,#8017,.T.);
#10360=ORIENTED_EDGE('',*,*,#8020,.T.);
#10361=ORIENTED_EDGE('',*,*,#8023,.T.);
#10362=ORIENTED_EDGE('',*,*,#8026,.T.);
#10363=ORIENTED_EDGE('',*,*,#8029,.T.);
#10364=ORIENTED_EDGE('',*,*,#8032,.T.);
#10365=ORIENTED_EDGE('',*,*,#8035,.T.);
#10366=ORIENTED_EDGE('',*,*,#8038,.T.);
#10367=ORIENTED_EDGE('',*,*,#8041,.T.);
#10368=ORIENTED_EDGE('',*,*,#8044,.T.);
#10369=ORIENTED_EDGE('',*,*,#8047,.T.);
#10370=ORIENTED_EDGE('',*,*,#8050,.T.);
#10371=ORIENTED_EDGE('',*,*,#8053,.T.);
#10372=ORIENTED_EDGE('',*,*,#8056,.T.);
#10373=ORIENTED_EDGE('',*,*,#8059,.T.);
#10374=ORIENTED_EDGE('',*,*,#8062,.T.);
#10375=ORIENTED_EDGE('',*,*,#8065,.T.);
#10376=ORIENTED_EDGE('',*,*,#8068,.T.);
#10377=ORIENTED_EDGE('',*,*,#8071,.T.);
#10378=ORIENTED_EDGE('',*,*,#8081,.T.);
#10379=ORIENTED_EDGE('',*,*,#8078,.T.);
#10380=ORIENTED_EDGE('',*,*,#8075,.T.);
#10381=ORIENTED_EDGE('',*,*,#8019,.F.);
#10382=ORIENTED_EDGE('',*,*,#8022,.F.);
#10383=ORIENTED_EDGE('',*,*,#8025,.F.);
#10384=ORIENTED_EDGE('',*,*,#8028,.F.);
#10385=ORIENTED_EDGE('',*,*,#8031,.F.);
#10386=ORIENTED_EDGE('',*,*,#8034,.F.);
#10387=ORIENTED_EDGE('',*,*,#8037,.F.);
#10388=ORIENTED_EDGE('',*,*,#8040,.F.);
#10389=ORIENTED_EDGE('',*,*,#8043,.F.);
#10390=ORIENTED_EDGE('',*,*,#8046,.F.);
#10391=ORIENTED_EDGE('',*,*,#8049,.F.);
#10392=ORIENTED_EDGE('',*,*,#8052,.F.);
#10393=ORIENTED_EDGE('',*,*,#8055,.F.);
#10394=ORIENTED_EDGE('',*,*,#8058,.F.);
#10395=ORIENTED_EDGE('',*,*,#8061,.F.);
#10396=ORIENTED_EDGE('',*,*,#8064,.F.);
#10397=ORIENTED_EDGE('',*,*,#8067,.F.);
#10398=ORIENTED_EDGE('',*,*,#8070,.F.);
#10399=ORIENTED_EDGE('',*,*,#8083,.T.);
#10400=ORIENTED_EDGE('',*,*,#8084,.T.);
#10401=ORIENTED_EDGE('',*,*,#8085,.F.);
#10402=ORIENTED_EDGE('',*,*,#8084,.F.);
#10403=ORIENTED_EDGE('',*,*,#8086,.T.);
#10404=ORIENTED_EDGE('',*,*,#8087,.T.);
#10405=ORIENTED_EDGE('',*,*,#8088,.F.);
#10406=ORIENTED_EDGE('',*,*,#8087,.F.);
#10407=ORIENTED_EDGE('',*,*,#8085,.T.);
#10408=ORIENTED_EDGE('',*,*,#8086,.F.);
#10409=ORIENTED_EDGE('',*,*,#8083,.F.);
#10410=ORIENTED_EDGE('',*,*,#8088,.T.);
#10411=ORIENTED_EDGE('',*,*,#8089,.T.);
#10412=ORIENTED_EDGE('',*,*,#8090,.T.);
#10413=ORIENTED_EDGE('',*,*,#8091,.F.);
#10414=ORIENTED_EDGE('',*,*,#8090,.F.);
#10415=ORIENTED_EDGE('',*,*,#8092,.T.);
#10416=ORIENTED_EDGE('',*,*,#8093,.T.);
#10417=ORIENTED_EDGE('',*,*,#8094,.F.);
#10418=ORIENTED_EDGE('',*,*,#8093,.F.);
#10419=ORIENTED_EDGE('',*,*,#8091,.T.);
#10420=ORIENTED_EDGE('',*,*,#8092,.F.);
#10421=ORIENTED_EDGE('',*,*,#8089,.F.);
#10422=ORIENTED_EDGE('',*,*,#8094,.T.);
#10423=ORIENTED_EDGE('',*,*,#8095,.F.);
#10424=ORIENTED_EDGE('',*,*,#8096,.T.);
#10425=ORIENTED_EDGE('',*,*,#8097,.T.);
#10426=ORIENTED_EDGE('',*,*,#8096,.F.);
#10427=ORIENTED_EDGE('',*,*,#8098,.F.);
#10428=ORIENTED_EDGE('',*,*,#8099,.T.);
#10429=ORIENTED_EDGE('',*,*,#8100,.T.);
#10430=ORIENTED_EDGE('',*,*,#8099,.F.);
#10431=ORIENTED_EDGE('',*,*,#8101,.F.);
#10432=ORIENTED_EDGE('',*,*,#8102,.T.);
#10433=ORIENTED_EDGE('',*,*,#8103,.T.);
#10434=ORIENTED_EDGE('',*,*,#8102,.F.);
#10435=ORIENTED_EDGE('',*,*,#8104,.F.);
#10436=ORIENTED_EDGE('',*,*,#8105,.T.);
#10437=ORIENTED_EDGE('',*,*,#8106,.T.);
#10438=ORIENTED_EDGE('',*,*,#8105,.F.);
#10439=ORIENTED_EDGE('',*,*,#8107,.F.);
#10440=ORIENTED_EDGE('',*,*,#8108,.T.);
#10441=ORIENTED_EDGE('',*,*,#8109,.T.);
#10442=ORIENTED_EDGE('',*,*,#8108,.F.);
#10443=ORIENTED_EDGE('',*,*,#8110,.F.);
#10444=ORIENTED_EDGE('',*,*,#8111,.T.);
#10445=ORIENTED_EDGE('',*,*,#8112,.T.);
#10446=ORIENTED_EDGE('',*,*,#8111,.F.);
#10447=ORIENTED_EDGE('',*,*,#8113,.F.);
#10448=ORIENTED_EDGE('',*,*,#8114,.T.);
#10449=ORIENTED_EDGE('',*,*,#8115,.T.);
#10450=ORIENTED_EDGE('',*,*,#8114,.F.);
#10451=ORIENTED_EDGE('',*,*,#8116,.F.);
#10452=ORIENTED_EDGE('',*,*,#8117,.T.);
#10453=ORIENTED_EDGE('',*,*,#8118,.T.);
#10454=ORIENTED_EDGE('',*,*,#8117,.F.);
#10455=ORIENTED_EDGE('',*,*,#8119,.F.);
#10456=ORIENTED_EDGE('',*,*,#8120,.T.);
#10457=ORIENTED_EDGE('',*,*,#8121,.T.);
#10458=ORIENTED_EDGE('',*,*,#8120,.F.);
#10459=ORIENTED_EDGE('',*,*,#8122,.F.);
#10460=ORIENTED_EDGE('',*,*,#8123,.T.);
#10461=ORIENTED_EDGE('',*,*,#8124,.T.);
#10462=ORIENTED_EDGE('',*,*,#8123,.F.);
#10463=ORIENTED_EDGE('',*,*,#8125,.F.);
#10464=ORIENTED_EDGE('',*,*,#8126,.T.);
#10465=ORIENTED_EDGE('',*,*,#8127,.T.);
#10466=ORIENTED_EDGE('',*,*,#8126,.F.);
#10467=ORIENTED_EDGE('',*,*,#8128,.F.);
#10468=ORIENTED_EDGE('',*,*,#8129,.T.);
#10469=ORIENTED_EDGE('',*,*,#8130,.T.);
#10470=ORIENTED_EDGE('',*,*,#8129,.F.);
#10471=ORIENTED_EDGE('',*,*,#8131,.F.);
#10472=ORIENTED_EDGE('',*,*,#8132,.T.);
#10473=ORIENTED_EDGE('',*,*,#8133,.T.);
#10474=ORIENTED_EDGE('',*,*,#8132,.F.);
#10475=ORIENTED_EDGE('',*,*,#8134,.F.);
#10476=ORIENTED_EDGE('',*,*,#8135,.T.);
#10477=ORIENTED_EDGE('',*,*,#8136,.T.);
#10478=ORIENTED_EDGE('',*,*,#8135,.F.);
#10479=ORIENTED_EDGE('',*,*,#8136,.F.);
#10480=ORIENTED_EDGE('',*,*,#8095,.T.);
#10481=ORIENTED_EDGE('',*,*,#8098,.T.);
#10482=ORIENTED_EDGE('',*,*,#8101,.T.);
#10483=ORIENTED_EDGE('',*,*,#8104,.T.);
#10484=ORIENTED_EDGE('',*,*,#8107,.T.);
#10485=ORIENTED_EDGE('',*,*,#8110,.T.);
#10486=ORIENTED_EDGE('',*,*,#8113,.T.);
#10487=ORIENTED_EDGE('',*,*,#8116,.T.);
#10488=ORIENTED_EDGE('',*,*,#8119,.T.);
#10489=ORIENTED_EDGE('',*,*,#8122,.T.);
#10490=ORIENTED_EDGE('',*,*,#8125,.T.);
#10491=ORIENTED_EDGE('',*,*,#8128,.T.);
#10492=ORIENTED_EDGE('',*,*,#8131,.T.);
#10493=ORIENTED_EDGE('',*,*,#8134,.T.);
#10494=ORIENTED_EDGE('',*,*,#8097,.F.);
#10495=ORIENTED_EDGE('',*,*,#8100,.F.);
#10496=ORIENTED_EDGE('',*,*,#8103,.F.);
#10497=ORIENTED_EDGE('',*,*,#8106,.F.);
#10498=ORIENTED_EDGE('',*,*,#8109,.F.);
#10499=ORIENTED_EDGE('',*,*,#8112,.F.);
#10500=ORIENTED_EDGE('',*,*,#8115,.F.);
#10501=ORIENTED_EDGE('',*,*,#8118,.F.);
#10502=ORIENTED_EDGE('',*,*,#8121,.F.);
#10503=ORIENTED_EDGE('',*,*,#8124,.F.);
#10504=ORIENTED_EDGE('',*,*,#8127,.F.);
#10505=ORIENTED_EDGE('',*,*,#8130,.F.);
#10506=ORIENTED_EDGE('',*,*,#8133,.F.);
#10507=ORIENTED_EDGE('',*,*,#8137,.F.);
#10508=ORIENTED_EDGE('',*,*,#8138,.T.);
#10509=ORIENTED_EDGE('',*,*,#8139,.T.);
#10510=ORIENTED_EDGE('',*,*,#8138,.F.);
#10511=ORIENTED_EDGE('',*,*,#8140,.F.);
#10512=ORIENTED_EDGE('',*,*,#8141,.T.);
#10513=ORIENTED_EDGE('',*,*,#8142,.T.);
#10514=ORIENTED_EDGE('',*,*,#8141,.F.);
#10515=ORIENTED_EDGE('',*,*,#8143,.F.);
#10516=ORIENTED_EDGE('',*,*,#8144,.T.);
#10517=ORIENTED_EDGE('',*,*,#8145,.T.);
#10518=ORIENTED_EDGE('',*,*,#8144,.F.);
#10519=ORIENTED_EDGE('',*,*,#8146,.F.);
#10520=ORIENTED_EDGE('',*,*,#8147,.T.);
#10521=ORIENTED_EDGE('',*,*,#8148,.T.);
#10522=ORIENTED_EDGE('',*,*,#8147,.F.);
#10523=ORIENTED_EDGE('',*,*,#8149,.F.);
#10524=ORIENTED_EDGE('',*,*,#8150,.T.);
#10525=ORIENTED_EDGE('',*,*,#8151,.T.);
#10526=ORIENTED_EDGE('',*,*,#8150,.F.);
#10527=ORIENTED_EDGE('',*,*,#8152,.F.);
#10528=ORIENTED_EDGE('',*,*,#8153,.T.);
#10529=ORIENTED_EDGE('',*,*,#8154,.T.);
#10530=ORIENTED_EDGE('',*,*,#8153,.F.);
#10531=ORIENTED_EDGE('',*,*,#8154,.F.);
#10532=ORIENTED_EDGE('',*,*,#8137,.T.);
#10533=ORIENTED_EDGE('',*,*,#8140,.T.);
#10534=ORIENTED_EDGE('',*,*,#8143,.T.);
#10535=ORIENTED_EDGE('',*,*,#8146,.T.);
#10536=ORIENTED_EDGE('',*,*,#8149,.T.);
#10537=ORIENTED_EDGE('',*,*,#8152,.T.);
#10538=ORIENTED_EDGE('',*,*,#8139,.F.);
#10539=ORIENTED_EDGE('',*,*,#8142,.F.);
#10540=ORIENTED_EDGE('',*,*,#8145,.F.);
#10541=ORIENTED_EDGE('',*,*,#8148,.F.);
#10542=ORIENTED_EDGE('',*,*,#8151,.F.);
#10543=ORIENTED_EDGE('',*,*,#8155,.F.);
#10544=ORIENTED_EDGE('',*,*,#8156,.F.);
#10545=ORIENTED_EDGE('',*,*,#8157,.F.);
#10546=ORIENTED_EDGE('',*,*,#8158,.F.);
#10547=ORIENTED_EDGE('',*,*,#8159,.F.);
#10548=ORIENTED_EDGE('',*,*,#8160,.F.);
#10549=ORIENTED_EDGE('',*,*,#8161,.F.);
#10550=ORIENTED_EDGE('',*,*,#8162,.F.);
#10551=ORIENTED_EDGE('',*,*,#8163,.F.);
#10552=ORIENTED_EDGE('',*,*,#8164,.F.);
#10553=ORIENTED_EDGE('',*,*,#8165,.F.);
#10554=ORIENTED_EDGE('',*,*,#8166,.F.);
#10555=ORIENTED_EDGE('',*,*,#8167,.F.);
#10556=ORIENTED_EDGE('',*,*,#8168,.F.);
#10557=ORIENTED_EDGE('',*,*,#8169,.F.);
#10558=ORIENTED_EDGE('',*,*,#8170,.F.);
#10559=ORIENTED_EDGE('',*,*,#8171,.F.);
#10560=ORIENTED_EDGE('',*,*,#8172,.F.);
#10561=ORIENTED_EDGE('',*,*,#8173,.F.);
#10562=ORIENTED_EDGE('',*,*,#8156,.T.);
#10563=ORIENTED_EDGE('',*,*,#8174,.T.);
#10564=ORIENTED_EDGE('',*,*,#8164,.T.);
#10565=ORIENTED_EDGE('',*,*,#8175,.F.);
#10566=ORIENTED_EDGE('',*,*,#8157,.T.);
#10567=ORIENTED_EDGE('',*,*,#8173,.T.);
#10568=ORIENTED_EDGE('',*,*,#8172,.T.);
#10569=ORIENTED_EDGE('',*,*,#8176,.F.);
#10570=ORIENTED_EDGE('',*,*,#8158,.T.);
#10571=ORIENTED_EDGE('',*,*,#8175,.T.);
#10572=ORIENTED_EDGE('',*,*,#8171,.T.);
#10573=ORIENTED_EDGE('',*,*,#8177,.F.);
#10574=ORIENTED_EDGE('',*,*,#8159,.T.);
#10575=ORIENTED_EDGE('',*,*,#8176,.T.);
#10576=ORIENTED_EDGE('',*,*,#8170,.T.);
#10577=ORIENTED_EDGE('',*,*,#8178,.F.);
#10578=ORIENTED_EDGE('',*,*,#8160,.T.);
#10579=ORIENTED_EDGE('',*,*,#8177,.T.);
#10580=ORIENTED_EDGE('',*,*,#8169,.T.);
#10581=ORIENTED_EDGE('',*,*,#8179,.F.);
#10582=ORIENTED_EDGE('',*,*,#8161,.T.);
#10583=ORIENTED_EDGE('',*,*,#8178,.T.);
#10584=ORIENTED_EDGE('',*,*,#8168,.T.);
#10585=ORIENTED_EDGE('',*,*,#8180,.F.);
#10586=ORIENTED_EDGE('',*,*,#8162,.T.);
#10587=ORIENTED_EDGE('',*,*,#8179,.T.);
#10588=ORIENTED_EDGE('',*,*,#8167,.T.);
#10589=ORIENTED_EDGE('',*,*,#8181,.F.);
#10590=ORIENTED_EDGE('',*,*,#8163,.T.);
#10591=ORIENTED_EDGE('',*,*,#8180,.T.);
#10592=ORIENTED_EDGE('',*,*,#8166,.T.);
#10593=ORIENTED_EDGE('',*,*,#8174,.F.);
#10594=ORIENTED_EDGE('',*,*,#8155,.T.);
#10595=ORIENTED_EDGE('',*,*,#8181,.T.);
#10596=ORIENTED_EDGE('',*,*,#8165,.T.);
#10597=ORIENTED_EDGE('',*,*,#8182,.F.);
#10598=ORIENTED_EDGE('',*,*,#8183,.F.);
#10599=ORIENTED_EDGE('',*,*,#8184,.F.);
#10600=ORIENTED_EDGE('',*,*,#8185,.F.);
#10601=ORIENTED_EDGE('',*,*,#8186,.F.);
#10602=ORIENTED_EDGE('',*,*,#8187,.F.);
#10603=ORIENTED_EDGE('',*,*,#8188,.F.);
#10604=ORIENTED_EDGE('',*,*,#8189,.F.);
#10605=ORIENTED_EDGE('',*,*,#8190,.F.);
#10606=ORIENTED_EDGE('',*,*,#8191,.F.);
#10607=ORIENTED_EDGE('',*,*,#8192,.F.);
#10608=ORIENTED_EDGE('',*,*,#8193,.F.);
#10609=ORIENTED_EDGE('',*,*,#8194,.F.);
#10610=ORIENTED_EDGE('',*,*,#8195,.F.);
#10611=ORIENTED_EDGE('',*,*,#8196,.F.);
#10612=ORIENTED_EDGE('',*,*,#8197,.F.);
#10613=ORIENTED_EDGE('',*,*,#8198,.F.);
#10614=ORIENTED_EDGE('',*,*,#8199,.F.);
#10615=ORIENTED_EDGE('',*,*,#8200,.T.);
#10616=ORIENTED_EDGE('',*,*,#8190,.T.);
#10617=ORIENTED_EDGE('',*,*,#8201,.F.);
#10618=ORIENTED_EDGE('',*,*,#8191,.T.);
#10619=ORIENTED_EDGE('',*,*,#8201,.T.);
#10620=ORIENTED_EDGE('',*,*,#8189,.T.);
#10621=ORIENTED_EDGE('',*,*,#8202,.F.);
#10622=ORIENTED_EDGE('',*,*,#8192,.T.);
#10623=ORIENTED_EDGE('',*,*,#8202,.T.);
#10624=ORIENTED_EDGE('',*,*,#8188,.T.);
#10625=ORIENTED_EDGE('',*,*,#8203,.F.);
#10626=ORIENTED_EDGE('',*,*,#8193,.T.);
#10627=ORIENTED_EDGE('',*,*,#8203,.T.);
#10628=ORIENTED_EDGE('',*,*,#8187,.T.);
#10629=ORIENTED_EDGE('',*,*,#8204,.F.);
#10630=ORIENTED_EDGE('',*,*,#8194,.T.);
#10631=ORIENTED_EDGE('',*,*,#8204,.T.);
#10632=ORIENTED_EDGE('',*,*,#8186,.T.);
#10633=ORIENTED_EDGE('',*,*,#8205,.F.);
#10634=ORIENTED_EDGE('',*,*,#8195,.T.);
#10635=ORIENTED_EDGE('',*,*,#8205,.T.);
#10636=ORIENTED_EDGE('',*,*,#8185,.T.);
#10637=ORIENTED_EDGE('',*,*,#8206,.F.);
#10638=ORIENTED_EDGE('',*,*,#8196,.T.);
#10639=ORIENTED_EDGE('',*,*,#8206,.T.);
#10640=ORIENTED_EDGE('',*,*,#8184,.T.);
#10641=ORIENTED_EDGE('',*,*,#8207,.F.);
#10642=ORIENTED_EDGE('',*,*,#8197,.T.);
#10643=ORIENTED_EDGE('',*,*,#8207,.T.);
#10644=ORIENTED_EDGE('',*,*,#8183,.T.);
#10645=ORIENTED_EDGE('',*,*,#8208,.F.);
#10646=ORIENTED_EDGE('',*,*,#8198,.T.);
#10647=ORIENTED_EDGE('',*,*,#8208,.T.);
#10648=ORIENTED_EDGE('',*,*,#8182,.T.);
#10649=ORIENTED_EDGE('',*,*,#8200,.F.);
#10650=ORIENTED_EDGE('',*,*,#8199,.T.);
#10651=ORIENTED_EDGE('',*,*,#8209,.F.);
#10652=ORIENTED_EDGE('',*,*,#8210,.F.);
#10653=ORIENTED_EDGE('',*,*,#8211,.F.);
#10654=ORIENTED_EDGE('',*,*,#8212,.F.);
#10655=ORIENTED_EDGE('',*,*,#8213,.F.);
#10656=ORIENTED_EDGE('',*,*,#8214,.F.);
#10657=ORIENTED_EDGE('',*,*,#8215,.F.);
#10658=ORIENTED_EDGE('',*,*,#8216,.F.);
#10659=ORIENTED_EDGE('',*,*,#8217,.F.);
#10660=ORIENTED_EDGE('',*,*,#8218,.F.);
#10661=ORIENTED_EDGE('',*,*,#8219,.F.);
#10662=ORIENTED_EDGE('',*,*,#8220,.F.);
#10663=ORIENTED_EDGE('',*,*,#8221,.F.);
#10664=ORIENTED_EDGE('',*,*,#8222,.F.);
#10665=ORIENTED_EDGE('',*,*,#8223,.F.);
#10666=ORIENTED_EDGE('',*,*,#8224,.F.);
#10667=ORIENTED_EDGE('',*,*,#8225,.F.);
#10668=ORIENTED_EDGE('',*,*,#8226,.F.);
#10669=ORIENTED_EDGE('',*,*,#8227,.T.);
#10670=ORIENTED_EDGE('',*,*,#8217,.T.);
#10671=ORIENTED_EDGE('',*,*,#8228,.F.);
#10672=ORIENTED_EDGE('',*,*,#8218,.T.);
#10673=ORIENTED_EDGE('',*,*,#8228,.T.);
#10674=ORIENTED_EDGE('',*,*,#8216,.T.);
#10675=ORIENTED_EDGE('',*,*,#8229,.F.);
#10676=ORIENTED_EDGE('',*,*,#8219,.T.);
#10677=ORIENTED_EDGE('',*,*,#8229,.T.);
#10678=ORIENTED_EDGE('',*,*,#8215,.T.);
#10679=ORIENTED_EDGE('',*,*,#8230,.F.);
#10680=ORIENTED_EDGE('',*,*,#8220,.T.);
#10681=ORIENTED_EDGE('',*,*,#8230,.T.);
#10682=ORIENTED_EDGE('',*,*,#8214,.T.);
#10683=ORIENTED_EDGE('',*,*,#8231,.F.);
#10684=ORIENTED_EDGE('',*,*,#8221,.T.);
#10685=ORIENTED_EDGE('',*,*,#8231,.T.);
#10686=ORIENTED_EDGE('',*,*,#8213,.T.);
#10687=ORIENTED_EDGE('',*,*,#8232,.F.);
#10688=ORIENTED_EDGE('',*,*,#8222,.T.);
#10689=ORIENTED_EDGE('',*,*,#8232,.T.);
#10690=ORIENTED_EDGE('',*,*,#8212,.T.);
#10691=ORIENTED_EDGE('',*,*,#8233,.F.);
#10692=ORIENTED_EDGE('',*,*,#8223,.T.);
#10693=ORIENTED_EDGE('',*,*,#8233,.T.);
#10694=ORIENTED_EDGE('',*,*,#8211,.T.);
#10695=ORIENTED_EDGE('',*,*,#8234,.F.);
#10696=ORIENTED_EDGE('',*,*,#8224,.T.);
#10697=ORIENTED_EDGE('',*,*,#8234,.T.);
#10698=ORIENTED_EDGE('',*,*,#8210,.T.);
#10699=ORIENTED_EDGE('',*,*,#8235,.F.);
#10700=ORIENTED_EDGE('',*,*,#8225,.T.);
#10701=ORIENTED_EDGE('',*,*,#8235,.T.);
#10702=ORIENTED_EDGE('',*,*,#8209,.T.);
#10703=ORIENTED_EDGE('',*,*,#8227,.F.);
#10704=ORIENTED_EDGE('',*,*,#8226,.T.);
#10705=ORIENTED_EDGE('',*,*,#8236,.F.);
#10706=ORIENTED_EDGE('',*,*,#8237,.T.);
#10707=ORIENTED_EDGE('',*,*,#8238,.T.);
#10708=ORIENTED_EDGE('',*,*,#8237,.F.);
#10709=ORIENTED_EDGE('',*,*,#8239,.T.);
#10710=ORIENTED_EDGE('',*,*,#8240,.T.);
#10711=ORIENTED_EDGE('',*,*,#8241,.F.);
#10712=ORIENTED_EDGE('',*,*,#8242,.F.);
#10713=ORIENTED_EDGE('',*,*,#8243,.F.);
#10714=ORIENTED_EDGE('',*,*,#8244,.F.);
#10715=ORIENTED_EDGE('',*,*,#8245,.T.);
#10716=ORIENTED_EDGE('',*,*,#8242,.T.);
#10717=ORIENTED_EDGE('',*,*,#8246,.F.);
#10718=ORIENTED_EDGE('',*,*,#8247,.F.);
#10719=ORIENTED_EDGE('',*,*,#8248,.T.);
#10720=ORIENTED_EDGE('',*,*,#8244,.T.);
#10721=ORIENTED_EDGE('',*,*,#8249,.F.);
#10722=ORIENTED_EDGE('',*,*,#8250,.F.);
#10723=ORIENTED_EDGE('',*,*,#8251,.T.);
#10724=ORIENTED_EDGE('',*,*,#8247,.T.);
#10725=ORIENTED_EDGE('',*,*,#8252,.F.);
#10726=ORIENTED_EDGE('',*,*,#8253,.F.);
#10727=ORIENTED_EDGE('',*,*,#8254,.T.);
#10728=ORIENTED_EDGE('',*,*,#8250,.T.);
#10729=ORIENTED_EDGE('',*,*,#8255,.F.);
#10730=ORIENTED_EDGE('',*,*,#8240,.F.);
#10731=ORIENTED_EDGE('',*,*,#8256,.T.);
#10732=ORIENTED_EDGE('',*,*,#8253,.T.);
#10733=ORIENTED_EDGE('',*,*,#8239,.F.);
#10734=ORIENTED_EDGE('',*,*,#8245,.F.);
#10735=ORIENTED_EDGE('',*,*,#8248,.F.);
#10736=ORIENTED_EDGE('',*,*,#8251,.F.);
#10737=ORIENTED_EDGE('',*,*,#8254,.F.);
#10738=ORIENTED_EDGE('',*,*,#8256,.F.);
#10739=ORIENTED_EDGE('',*,*,#8236,.T.);
#10740=ORIENTED_EDGE('',*,*,#8241,.T.);
#10741=ORIENTED_EDGE('',*,*,#8255,.T.);
#10742=ORIENTED_EDGE('',*,*,#8252,.T.);
#10743=ORIENTED_EDGE('',*,*,#8249,.T.);
#10744=ORIENTED_EDGE('',*,*,#8246,.T.);
#10745=ORIENTED_EDGE('',*,*,#8243,.T.);
#10746=ORIENTED_EDGE('',*,*,#8238,.F.);
#10747=ORIENTED_EDGE('',*,*,#8257,.T.);
#10748=ORIENTED_EDGE('',*,*,#8258,.T.);
#10749=ORIENTED_EDGE('',*,*,#8259,.F.);
#10750=ORIENTED_EDGE('',*,*,#8258,.F.);
#10751=ORIENTED_EDGE('',*,*,#8260,.T.);
#10752=ORIENTED_EDGE('',*,*,#8261,.T.);
#10753=ORIENTED_EDGE('',*,*,#8262,.T.);
#10754=ORIENTED_EDGE('',*,*,#8263,.T.);
#10755=ORIENTED_EDGE('',*,*,#8264,.T.);
#10756=ORIENTED_EDGE('',*,*,#8265,.T.);
#10757=ORIENTED_EDGE('',*,*,#8257,.F.);
#10758=ORIENTED_EDGE('',*,*,#8266,.F.);
#10759=ORIENTED_EDGE('',*,*,#8267,.F.);
#10760=ORIENTED_EDGE('',*,*,#8268,.F.);
#10761=ORIENTED_EDGE('',*,*,#8269,.F.);
#10762=ORIENTED_EDGE('',*,*,#8270,.F.);
#10763=ORIENTED_EDGE('',*,*,#8271,.F.);
#10764=ORIENTED_EDGE('',*,*,#8259,.T.);
#10765=ORIENTED_EDGE('',*,*,#8266,.T.);
#10766=ORIENTED_EDGE('',*,*,#8272,.F.);
#10767=ORIENTED_EDGE('',*,*,#8260,.F.);
#10768=ORIENTED_EDGE('',*,*,#8273,.T.);
#10769=ORIENTED_EDGE('',*,*,#8271,.T.);
#10770=ORIENTED_EDGE('',*,*,#8274,.F.);
#10771=ORIENTED_EDGE('',*,*,#8261,.F.);
#10772=ORIENTED_EDGE('',*,*,#8272,.T.);
#10773=ORIENTED_EDGE('',*,*,#8270,.T.);
#10774=ORIENTED_EDGE('',*,*,#8275,.F.);
#10775=ORIENTED_EDGE('',*,*,#8262,.F.);
#10776=ORIENTED_EDGE('',*,*,#8274,.T.);
#10777=ORIENTED_EDGE('',*,*,#8269,.T.);
#10778=ORIENTED_EDGE('',*,*,#8276,.F.);
#10779=ORIENTED_EDGE('',*,*,#8263,.F.);
#10780=ORIENTED_EDGE('',*,*,#8275,.T.);
#10781=ORIENTED_EDGE('',*,*,#8268,.T.);
#10782=ORIENTED_EDGE('',*,*,#8277,.F.);
#10783=ORIENTED_EDGE('',*,*,#8264,.F.);
#10784=ORIENTED_EDGE('',*,*,#8276,.T.);
#10785=ORIENTED_EDGE('',*,*,#8267,.T.);
#10786=ORIENTED_EDGE('',*,*,#8273,.F.);
#10787=ORIENTED_EDGE('',*,*,#8265,.F.);
#10788=ORIENTED_EDGE('',*,*,#8277,.T.);
#10789=ORIENTED_EDGE('',*,*,#8278,.T.);
#10790=ORIENTED_EDGE('',*,*,#8279,.T.);
#10791=ORIENTED_EDGE('',*,*,#8280,.F.);
#10792=ORIENTED_EDGE('',*,*,#8279,.F.);
#10793=ORIENTED_EDGE('',*,*,#8281,.F.);
#10794=ORIENTED_EDGE('',*,*,#8282,.T.);
#10795=ORIENTED_EDGE('',*,*,#8283,.T.);
#10796=ORIENTED_EDGE('',*,*,#8284,.F.);
#10797=ORIENTED_EDGE('',*,*,#8285,.T.);
#10798=ORIENTED_EDGE('',*,*,#8282,.F.);
#10799=ORIENTED_EDGE('',*,*,#8286,.F.);
#10800=ORIENTED_EDGE('',*,*,#8287,.T.);
#10801=ORIENTED_EDGE('',*,*,#8288,.T.);
#10802=ORIENTED_EDGE('',*,*,#8287,.F.);
#10803=ORIENTED_EDGE('',*,*,#8289,.F.);
#10804=ORIENTED_EDGE('',*,*,#8290,.T.);
#10805=ORIENTED_EDGE('',*,*,#8291,.T.);
#10806=ORIENTED_EDGE('',*,*,#8290,.F.);
#10807=ORIENTED_EDGE('',*,*,#8292,.F.);
#10808=ORIENTED_EDGE('',*,*,#8293,.T.);
#10809=ORIENTED_EDGE('',*,*,#8294,.T.);
#10810=ORIENTED_EDGE('',*,*,#8293,.F.);
#10811=ORIENTED_EDGE('',*,*,#8295,.F.);
#10812=ORIENTED_EDGE('',*,*,#8296,.T.);
#10813=ORIENTED_EDGE('',*,*,#8297,.T.);
#10814=ORIENTED_EDGE('',*,*,#8296,.F.);
#10815=ORIENTED_EDGE('',*,*,#8298,.F.);
#10816=ORIENTED_EDGE('',*,*,#8284,.T.);
#10817=ORIENTED_EDGE('',*,*,#8281,.T.);
#10818=ORIENTED_EDGE('',*,*,#8298,.T.);
#10819=ORIENTED_EDGE('',*,*,#8295,.T.);
#10820=ORIENTED_EDGE('',*,*,#8292,.T.);
#10821=ORIENTED_EDGE('',*,*,#8289,.T.);
#10822=ORIENTED_EDGE('',*,*,#8286,.T.);
#10823=ORIENTED_EDGE('',*,*,#8278,.F.);
#10824=ORIENTED_EDGE('',*,*,#8283,.F.);
#10825=ORIENTED_EDGE('',*,*,#8285,.F.);
#10826=ORIENTED_EDGE('',*,*,#8288,.F.);
#10827=ORIENTED_EDGE('',*,*,#8291,.F.);
#10828=ORIENTED_EDGE('',*,*,#8294,.F.);
#10829=ORIENTED_EDGE('',*,*,#8297,.F.);
#10830=ORIENTED_EDGE('',*,*,#8280,.T.);
#10831=ORIENTED_EDGE('',*,*,#8299,.F.);
#10832=ORIENTED_EDGE('',*,*,#8300,.T.);
#10833=ORIENTED_EDGE('',*,*,#8301,.T.);
#10834=ORIENTED_EDGE('',*,*,#8300,.F.);
#10835=ORIENTED_EDGE('',*,*,#8302,.F.);
#10836=ORIENTED_EDGE('',*,*,#8303,.F.);
#10837=ORIENTED_EDGE('',*,*,#8304,.F.);
#10838=ORIENTED_EDGE('',*,*,#8305,.F.);
#10839=ORIENTED_EDGE('',*,*,#8306,.F.);
#10840=ORIENTED_EDGE('',*,*,#8307,.F.);
#10841=ORIENTED_EDGE('',*,*,#8299,.T.);
#10842=ORIENTED_EDGE('',*,*,#8308,.T.);
#10843=ORIENTED_EDGE('',*,*,#8309,.T.);
#10844=ORIENTED_EDGE('',*,*,#8310,.T.);
#10845=ORIENTED_EDGE('',*,*,#8311,.T.);
#10846=ORIENTED_EDGE('',*,*,#8312,.T.);
#10847=ORIENTED_EDGE('',*,*,#8313,.T.);
#10848=ORIENTED_EDGE('',*,*,#8301,.F.);
#10849=ORIENTED_EDGE('',*,*,#8308,.F.);
#10850=ORIENTED_EDGE('',*,*,#8314,.F.);
#10851=ORIENTED_EDGE('',*,*,#8302,.T.);
#10852=ORIENTED_EDGE('',*,*,#8315,.T.);
#10853=ORIENTED_EDGE('',*,*,#8309,.F.);
#10854=ORIENTED_EDGE('',*,*,#8315,.F.);
#10855=ORIENTED_EDGE('',*,*,#8307,.T.);
#10856=ORIENTED_EDGE('',*,*,#8316,.T.);
#10857=ORIENTED_EDGE('',*,*,#8310,.F.);
#10858=ORIENTED_EDGE('',*,*,#8316,.F.);
#10859=ORIENTED_EDGE('',*,*,#8306,.T.);
#10860=ORIENTED_EDGE('',*,*,#8317,.T.);
#10861=ORIENTED_EDGE('',*,*,#8311,.F.);
#10862=ORIENTED_EDGE('',*,*,#8317,.F.);
#10863=ORIENTED_EDGE('',*,*,#8305,.T.);
#10864=ORIENTED_EDGE('',*,*,#8318,.T.);
#10865=ORIENTED_EDGE('',*,*,#8312,.F.);
#10866=ORIENTED_EDGE('',*,*,#8318,.F.);
#10867=ORIENTED_EDGE('',*,*,#8304,.T.);
#10868=ORIENTED_EDGE('',*,*,#8319,.T.);
#10869=ORIENTED_EDGE('',*,*,#8313,.F.);
#10870=ORIENTED_EDGE('',*,*,#8319,.F.);
#10871=ORIENTED_EDGE('',*,*,#8303,.T.);
#10872=ORIENTED_EDGE('',*,*,#8314,.T.);
#10873=ORIENTED_EDGE('',*,*,#8320,.T.);
#10874=ORIENTED_EDGE('',*,*,#8321,.T.);
#10875=ORIENTED_EDGE('',*,*,#8322,.T.);
#10876=ORIENTED_EDGE('',*,*,#8323,.F.);
#10877=ORIENTED_EDGE('',*,*,#8324,.T.);
#10878=ORIENTED_EDGE('',*,*,#8325,.T.);
#10879=ORIENTED_EDGE('',*,*,#8326,.T.);
#10880=ORIENTED_EDGE('',*,*,#8327,.F.);
#10881=ORIENTED_EDGE('',*,*,#8328,.F.);
#10882=ORIENTED_EDGE('',*,*,#8329,.F.);
#10883=ORIENTED_EDGE('',*,*,#8330,.F.);
#10884=ORIENTED_EDGE('',*,*,#8331,.T.);
#10885=ORIENTED_EDGE('',*,*,#8332,.F.);
#10886=ORIENTED_EDGE('',*,*,#8333,.F.);
#10887=ORIENTED_EDGE('',*,*,#8334,.T.);
#10888=ORIENTED_EDGE('',*,*,#8335,.T.);
#10889=ORIENTED_EDGE('',*,*,#8336,.F.);
#10890=ORIENTED_EDGE('',*,*,#8337,.F.);
#10891=ORIENTED_EDGE('',*,*,#8338,.F.);
#10892=ORIENTED_EDGE('',*,*,#8329,.T.);
#10893=ORIENTED_EDGE('',*,*,#8339,.F.);
#10894=ORIENTED_EDGE('',*,*,#8340,.F.);
#10895=ORIENTED_EDGE('',*,*,#8341,.T.);
#10896=ORIENTED_EDGE('',*,*,#8333,.T.);
#10897=ORIENTED_EDGE('',*,*,#8342,.F.);
#10898=ORIENTED_EDGE('',*,*,#8343,.F.);
#10899=ORIENTED_EDGE('',*,*,#8344,.F.);
#10900=ORIENTED_EDGE('',*,*,#8345,.F.);
#10901=ORIENTED_EDGE('',*,*,#8346,.F.);
#10902=ORIENTED_EDGE('',*,*,#8347,.F.);
#10903=ORIENTED_EDGE('',*,*,#8348,.F.);
#10904=ORIENTED_EDGE('',*,*,#8349,.F.);
#10905=ORIENTED_EDGE('',*,*,#8350,.F.);
#10906=ORIENTED_EDGE('',*,*,#8351,.F.);
#10907=ORIENTED_EDGE('',*,*,#8352,.F.);
#10908=ORIENTED_EDGE('',*,*,#8353,.F.);
#10909=ORIENTED_EDGE('',*,*,#8354,.F.);
#10910=ORIENTED_EDGE('',*,*,#8355,.F.);
#10911=ORIENTED_EDGE('',*,*,#8356,.F.);
#10912=ORIENTED_EDGE('',*,*,#8357,.F.);
#10913=ORIENTED_EDGE('',*,*,#8334,.F.);
#10914=ORIENTED_EDGE('',*,*,#8341,.F.);
#10915=ORIENTED_EDGE('',*,*,#8358,.F.);
#10916=ORIENTED_EDGE('',*,*,#8322,.F.);
#10917=ORIENTED_EDGE('',*,*,#8359,.F.);
#10918=ORIENTED_EDGE('',*,*,#8360,.T.);
#10919=ORIENTED_EDGE('',*,*,#8350,.T.);
#10920=ORIENTED_EDGE('',*,*,#8361,.F.);
#10921=ORIENTED_EDGE('',*,*,#8351,.T.);
#10922=ORIENTED_EDGE('',*,*,#8340,.T.);
#10923=ORIENTED_EDGE('',*,*,#8362,.F.);
#10924=ORIENTED_EDGE('',*,*,#8326,.F.);
#10925=ORIENTED_EDGE('',*,*,#8363,.F.);
#10926=ORIENTED_EDGE('',*,*,#8337,.T.);
#10927=ORIENTED_EDGE('',*,*,#8361,.T.);
#10928=ORIENTED_EDGE('',*,*,#8349,.T.);
#10929=ORIENTED_EDGE('',*,*,#8364,.F.);
#10930=ORIENTED_EDGE('',*,*,#8352,.T.);
#10931=ORIENTED_EDGE('',*,*,#8364,.T.);
#10932=ORIENTED_EDGE('',*,*,#8348,.T.);
#10933=ORIENTED_EDGE('',*,*,#8365,.F.);
#10934=ORIENTED_EDGE('',*,*,#8353,.T.);
#10935=ORIENTED_EDGE('',*,*,#8365,.T.);
#10936=ORIENTED_EDGE('',*,*,#8347,.T.);
#10937=ORIENTED_EDGE('',*,*,#8366,.F.);
#10938=ORIENTED_EDGE('',*,*,#8354,.T.);
#10939=ORIENTED_EDGE('',*,*,#8366,.T.);
#10940=ORIENTED_EDGE('',*,*,#8346,.T.);
#10941=ORIENTED_EDGE('',*,*,#8367,.F.);
#10942=ORIENTED_EDGE('',*,*,#8355,.T.);
#10943=ORIENTED_EDGE('',*,*,#8367,.T.);
#10944=ORIENTED_EDGE('',*,*,#8345,.T.);
#10945=ORIENTED_EDGE('',*,*,#8368,.F.);
#10946=ORIENTED_EDGE('',*,*,#8356,.T.);
#10947=ORIENTED_EDGE('',*,*,#8369,.F.);
#10948=ORIENTED_EDGE('',*,*,#8331,.F.);
#10949=ORIENTED_EDGE('',*,*,#8370,.F.);
#10950=ORIENTED_EDGE('',*,*,#8324,.F.);
#10951=ORIENTED_EDGE('',*,*,#8371,.F.);
#10952=ORIENTED_EDGE('',*,*,#8335,.F.);
#10953=ORIENTED_EDGE('',*,*,#8357,.T.);
#10954=ORIENTED_EDGE('',*,*,#8368,.T.);
#10955=ORIENTED_EDGE('',*,*,#8344,.T.);
#10956=ORIENTED_EDGE('',*,*,#8372,.F.);
#10957=ORIENTED_EDGE('',*,*,#8373,.F.);
#10958=ORIENTED_EDGE('',*,*,#8320,.F.);
#10959=ORIENTED_EDGE('',*,*,#8374,.F.);
#10960=ORIENTED_EDGE('',*,*,#8372,.T.);
#10961=ORIENTED_EDGE('',*,*,#8343,.T.);
#10962=ORIENTED_EDGE('',*,*,#8375,.F.);
#10963=ORIENTED_EDGE('',*,*,#8376,.F.);
#10964=ORIENTED_EDGE('',*,*,#8375,.T.);
#10965=ORIENTED_EDGE('',*,*,#8342,.T.);
#10966=ORIENTED_EDGE('',*,*,#8360,.F.);
#10967=ORIENTED_EDGE('',*,*,#8371,.T.);
#10968=ORIENTED_EDGE('',*,*,#8327,.T.);
#10969=ORIENTED_EDGE('',*,*,#8362,.T.);
#10970=ORIENTED_EDGE('',*,*,#8339,.T.);
#10971=ORIENTED_EDGE('',*,*,#8332,.T.);
#10972=ORIENTED_EDGE('',*,*,#8370,.T.);
#10973=ORIENTED_EDGE('',*,*,#8330,.T.);
#10974=ORIENTED_EDGE('',*,*,#8338,.T.);
#10975=ORIENTED_EDGE('',*,*,#8363,.T.);
#10976=ORIENTED_EDGE('',*,*,#8325,.F.);
#10977=ORIENTED_EDGE('',*,*,#8369,.T.);
#10978=ORIENTED_EDGE('',*,*,#8323,.T.);
#10979=ORIENTED_EDGE('',*,*,#8358,.T.);
#10980=ORIENTED_EDGE('',*,*,#8336,.T.);
#10981=ORIENTED_EDGE('',*,*,#8328,.T.);
#10982=ORIENTED_EDGE('',*,*,#8373,.T.);
#10983=ORIENTED_EDGE('',*,*,#8374,.T.);
#10984=ORIENTED_EDGE('',*,*,#8376,.T.);
#10985=ORIENTED_EDGE('',*,*,#8359,.T.);
#10986=ORIENTED_EDGE('',*,*,#8321,.F.);
#10987=ORIENTED_EDGE('',*,*,#8377,.F.);
#10988=ORIENTED_EDGE('',*,*,#8378,.T.);
#10989=ORIENTED_EDGE('',*,*,#8379,.T.);
#10990=ORIENTED_EDGE('',*,*,#8378,.F.);
#10991=ORIENTED_EDGE('',*,*,#8380,.F.);
#10992=ORIENTED_EDGE('',*,*,#8381,.F.);
#10993=ORIENTED_EDGE('',*,*,#8382,.F.);
#10994=ORIENTED_EDGE('',*,*,#8383,.F.);
#10995=ORIENTED_EDGE('',*,*,#8384,.F.);
#10996=ORIENTED_EDGE('',*,*,#8385,.F.);
#10997=ORIENTED_EDGE('',*,*,#8377,.T.);
#10998=ORIENTED_EDGE('',*,*,#8386,.T.);
#10999=ORIENTED_EDGE('',*,*,#8387,.T.);
#11000=ORIENTED_EDGE('',*,*,#8388,.T.);
#11001=ORIENTED_EDGE('',*,*,#8389,.T.);
#11002=ORIENTED_EDGE('',*,*,#8390,.T.);
#11003=ORIENTED_EDGE('',*,*,#8391,.T.);
#11004=ORIENTED_EDGE('',*,*,#8379,.F.);
#11005=ORIENTED_EDGE('',*,*,#8386,.F.);
#11006=ORIENTED_EDGE('',*,*,#8392,.F.);
#11007=ORIENTED_EDGE('',*,*,#8380,.T.);
#11008=ORIENTED_EDGE('',*,*,#8393,.T.);
#11009=ORIENTED_EDGE('',*,*,#8387,.F.);
#11010=ORIENTED_EDGE('',*,*,#8393,.F.);
#11011=ORIENTED_EDGE('',*,*,#8385,.T.);
#11012=ORIENTED_EDGE('',*,*,#8394,.T.);
#11013=ORIENTED_EDGE('',*,*,#8388,.F.);
#11014=ORIENTED_EDGE('',*,*,#8394,.F.);
#11015=ORIENTED_EDGE('',*,*,#8384,.T.);
#11016=ORIENTED_EDGE('',*,*,#8395,.T.);
#11017=ORIENTED_EDGE('',*,*,#8389,.F.);
#11018=ORIENTED_EDGE('',*,*,#8395,.F.);
#11019=ORIENTED_EDGE('',*,*,#8383,.T.);
#11020=ORIENTED_EDGE('',*,*,#8396,.T.);
#11021=ORIENTED_EDGE('',*,*,#8390,.F.);
#11022=ORIENTED_EDGE('',*,*,#8396,.F.);
#11023=ORIENTED_EDGE('',*,*,#8382,.T.);
#11024=ORIENTED_EDGE('',*,*,#8397,.T.);
#11025=ORIENTED_EDGE('',*,*,#8391,.F.);
#11026=ORIENTED_EDGE('',*,*,#8397,.F.);
#11027=ORIENTED_EDGE('',*,*,#8381,.T.);
#11028=ORIENTED_EDGE('',*,*,#8392,.T.);
#11029=ORIENTED_EDGE('',*,*,#8398,.T.);
#11030=ORIENTED_EDGE('',*,*,#8399,.T.);
#11031=ORIENTED_EDGE('',*,*,#8400,.F.);
#11032=ORIENTED_EDGE('',*,*,#8399,.F.);
#11033=ORIENTED_EDGE('',*,*,#8401,.T.);
#11034=ORIENTED_EDGE('',*,*,#8402,.T.);
#11035=ORIENTED_EDGE('',*,*,#8403,.T.);
#11036=ORIENTED_EDGE('',*,*,#8404,.T.);
#11037=ORIENTED_EDGE('',*,*,#8405,.T.);
#11038=ORIENTED_EDGE('',*,*,#8406,.T.);
#11039=ORIENTED_EDGE('',*,*,#8398,.F.);
#11040=ORIENTED_EDGE('',*,*,#8407,.F.);
#11041=ORIENTED_EDGE('',*,*,#8408,.F.);
#11042=ORIENTED_EDGE('',*,*,#8409,.F.);
#11043=ORIENTED_EDGE('',*,*,#8410,.F.);
#11044=ORIENTED_EDGE('',*,*,#8411,.F.);
#11045=ORIENTED_EDGE('',*,*,#8412,.F.);
#11046=ORIENTED_EDGE('',*,*,#8400,.T.);
#11047=ORIENTED_EDGE('',*,*,#8407,.T.);
#11048=ORIENTED_EDGE('',*,*,#8413,.F.);
#11049=ORIENTED_EDGE('',*,*,#8401,.F.);
#11050=ORIENTED_EDGE('',*,*,#8414,.T.);
#11051=ORIENTED_EDGE('',*,*,#8412,.T.);
#11052=ORIENTED_EDGE('',*,*,#8415,.F.);
#11053=ORIENTED_EDGE('',*,*,#8402,.F.);
#11054=ORIENTED_EDGE('',*,*,#8413,.T.);
#11055=ORIENTED_EDGE('',*,*,#8411,.T.);
#11056=ORIENTED_EDGE('',*,*,#8416,.F.);
#11057=ORIENTED_EDGE('',*,*,#8403,.F.);
#11058=ORIENTED_EDGE('',*,*,#8415,.T.);
#11059=ORIENTED_EDGE('',*,*,#8410,.T.);
#11060=ORIENTED_EDGE('',*,*,#8417,.F.);
#11061=ORIENTED_EDGE('',*,*,#8404,.F.);
#11062=ORIENTED_EDGE('',*,*,#8416,.T.);
#11063=ORIENTED_EDGE('',*,*,#8409,.T.);
#11064=ORIENTED_EDGE('',*,*,#8418,.F.);
#11065=ORIENTED_EDGE('',*,*,#8405,.F.);
#11066=ORIENTED_EDGE('',*,*,#8417,.T.);
#11067=ORIENTED_EDGE('',*,*,#8408,.T.);
#11068=ORIENTED_EDGE('',*,*,#8414,.F.);
#11069=ORIENTED_EDGE('',*,*,#8406,.F.);
#11070=ORIENTED_EDGE('',*,*,#8418,.T.);
#11071=ORIENTED_EDGE('',*,*,#8419,.F.);
#11072=ORIENTED_EDGE('',*,*,#8420,.F.);
#11073=ORIENTED_EDGE('',*,*,#8421,.T.);
#11074=ORIENTED_EDGE('',*,*,#8422,.T.);
#11075=ORIENTED_EDGE('',*,*,#8423,.F.);
#11076=ORIENTED_EDGE('',*,*,#8424,.F.);
#11077=ORIENTED_EDGE('',*,*,#8425,.T.);
#11078=ORIENTED_EDGE('',*,*,#8420,.T.);
#11079=ORIENTED_EDGE('',*,*,#8426,.F.);
#11080=ORIENTED_EDGE('',*,*,#8427,.F.);
#11081=ORIENTED_EDGE('',*,*,#8428,.T.);
#11082=ORIENTED_EDGE('',*,*,#8424,.T.);
#11083=ORIENTED_EDGE('',*,*,#8429,.F.);
#11084=ORIENTED_EDGE('',*,*,#8430,.F.);
#11085=ORIENTED_EDGE('',*,*,#8431,.T.);
#11086=ORIENTED_EDGE('',*,*,#8427,.T.);
#11087=ORIENTED_EDGE('',*,*,#8432,.F.);
#11088=ORIENTED_EDGE('',*,*,#8433,.F.);
#11089=ORIENTED_EDGE('',*,*,#8434,.T.);
#11090=ORIENTED_EDGE('',*,*,#8430,.T.);
#11091=ORIENTED_EDGE('',*,*,#8435,.F.);
#11092=ORIENTED_EDGE('',*,*,#8436,.F.);
#11093=ORIENTED_EDGE('',*,*,#8437,.T.);
#11094=ORIENTED_EDGE('',*,*,#8433,.T.);
#11095=ORIENTED_EDGE('',*,*,#8438,.F.);
#11096=ORIENTED_EDGE('',*,*,#8439,.F.);
#11097=ORIENTED_EDGE('',*,*,#8440,.T.);
#11098=ORIENTED_EDGE('',*,*,#8436,.T.);
#11099=ORIENTED_EDGE('',*,*,#8441,.F.);
#11100=ORIENTED_EDGE('',*,*,#8442,.F.);
#11101=ORIENTED_EDGE('',*,*,#8443,.T.);
#11102=ORIENTED_EDGE('',*,*,#8439,.T.);
#11103=ORIENTED_EDGE('',*,*,#8444,.F.);
#11104=ORIENTED_EDGE('',*,*,#8445,.F.);
#11105=ORIENTED_EDGE('',*,*,#8446,.T.);
#11106=ORIENTED_EDGE('',*,*,#8442,.T.);
#11107=ORIENTED_EDGE('',*,*,#8447,.F.);
#11108=ORIENTED_EDGE('',*,*,#8448,.F.);
#11109=ORIENTED_EDGE('',*,*,#8449,.T.);
#11110=ORIENTED_EDGE('',*,*,#8445,.T.);
#11111=ORIENTED_EDGE('',*,*,#8450,.F.);
#11112=ORIENTED_EDGE('',*,*,#8451,.F.);
#11113=ORIENTED_EDGE('',*,*,#8452,.T.);
#11114=ORIENTED_EDGE('',*,*,#8448,.T.);
#11115=ORIENTED_EDGE('',*,*,#8453,.F.);
#11116=ORIENTED_EDGE('',*,*,#8422,.F.);
#11117=ORIENTED_EDGE('',*,*,#8454,.T.);
#11118=ORIENTED_EDGE('',*,*,#8451,.T.);
#11119=ORIENTED_EDGE('',*,*,#8421,.F.);
#11120=ORIENTED_EDGE('',*,*,#8425,.F.);
#11121=ORIENTED_EDGE('',*,*,#8428,.F.);
#11122=ORIENTED_EDGE('',*,*,#8431,.F.);
#11123=ORIENTED_EDGE('',*,*,#8434,.F.);
#11124=ORIENTED_EDGE('',*,*,#8437,.F.);
#11125=ORIENTED_EDGE('',*,*,#8440,.F.);
#11126=ORIENTED_EDGE('',*,*,#8443,.F.);
#11127=ORIENTED_EDGE('',*,*,#8446,.F.);
#11128=ORIENTED_EDGE('',*,*,#8449,.F.);
#11129=ORIENTED_EDGE('',*,*,#8452,.F.);
#11130=ORIENTED_EDGE('',*,*,#8454,.F.);
#11131=ORIENTED_EDGE('',*,*,#8419,.T.);
#11132=ORIENTED_EDGE('',*,*,#8453,.T.);
#11133=ORIENTED_EDGE('',*,*,#8450,.T.);
#11134=ORIENTED_EDGE('',*,*,#8447,.T.);
#11135=ORIENTED_EDGE('',*,*,#8444,.T.);
#11136=ORIENTED_EDGE('',*,*,#8441,.T.);
#11137=ORIENTED_EDGE('',*,*,#8438,.T.);
#11138=ORIENTED_EDGE('',*,*,#8435,.T.);
#11139=ORIENTED_EDGE('',*,*,#8432,.T.);
#11140=ORIENTED_EDGE('',*,*,#8429,.T.);
#11141=ORIENTED_EDGE('',*,*,#8426,.T.);
#11142=ORIENTED_EDGE('',*,*,#8423,.T.);
#11143=ORIENTED_EDGE('',*,*,#8455,.T.);
#11144=ORIENTED_EDGE('',*,*,#8456,.T.);
#11145=ORIENTED_EDGE('',*,*,#8457,.F.);
#11146=ORIENTED_EDGE('',*,*,#8456,.F.);
#11147=ORIENTED_EDGE('',*,*,#8458,.F.);
#11148=ORIENTED_EDGE('',*,*,#8459,.T.);
#11149=ORIENTED_EDGE('',*,*,#8460,.T.);
#11150=ORIENTED_EDGE('',*,*,#8461,.F.);
#11151=ORIENTED_EDGE('',*,*,#8462,.F.);
#11152=ORIENTED_EDGE('',*,*,#8463,.T.);
#11153=ORIENTED_EDGE('',*,*,#8464,.T.);
#11154=ORIENTED_EDGE('',*,*,#8459,.F.);
#11155=ORIENTED_EDGE('',*,*,#8462,.T.);
#11156=ORIENTED_EDGE('',*,*,#8458,.T.);
#11157=ORIENTED_EDGE('',*,*,#8465,.T.);
#11158=ORIENTED_EDGE('',*,*,#8466,.T.);
#11159=ORIENTED_EDGE('',*,*,#8467,.T.);
#11160=ORIENTED_EDGE('',*,*,#8468,.T.);
#11161=ORIENTED_EDGE('',*,*,#8455,.F.);
#11162=ORIENTED_EDGE('',*,*,#8464,.F.);
#11163=ORIENTED_EDGE('',*,*,#8469,.F.);
#11164=ORIENTED_EDGE('',*,*,#8470,.F.);
#11165=ORIENTED_EDGE('',*,*,#8471,.F.);
#11166=ORIENTED_EDGE('',*,*,#8472,.F.);
#11167=ORIENTED_EDGE('',*,*,#8460,.F.);
#11168=ORIENTED_EDGE('',*,*,#8457,.T.);
#11169=ORIENTED_EDGE('',*,*,#8472,.T.);
#11170=ORIENTED_EDGE('',*,*,#8473,.F.);
#11171=ORIENTED_EDGE('',*,*,#8465,.F.);
#11172=ORIENTED_EDGE('',*,*,#8461,.T.);
#11173=ORIENTED_EDGE('',*,*,#8471,.T.);
#11174=ORIENTED_EDGE('',*,*,#8474,.F.);
#11175=ORIENTED_EDGE('',*,*,#8466,.F.);
#11176=ORIENTED_EDGE('',*,*,#8473,.T.);
#11177=ORIENTED_EDGE('',*,*,#8470,.T.);
#11178=ORIENTED_EDGE('',*,*,#8475,.F.);
#11179=ORIENTED_EDGE('',*,*,#8467,.F.);
#11180=ORIENTED_EDGE('',*,*,#8474,.T.);
#11181=ORIENTED_EDGE('',*,*,#8469,.T.);
#11182=ORIENTED_EDGE('',*,*,#8463,.F.);
#11183=ORIENTED_EDGE('',*,*,#8468,.F.);
#11184=ORIENTED_EDGE('',*,*,#8475,.T.);
#11185=ORIENTED_EDGE('',*,*,#8476,.F.);
#11186=ORIENTED_EDGE('',*,*,#8477,.T.);
#11187=ORIENTED_EDGE('',*,*,#8478,.T.);
#11188=ORIENTED_EDGE('',*,*,#8477,.F.);
#11189=ORIENTED_EDGE('',*,*,#8479,.T.);
#11190=ORIENTED_EDGE('',*,*,#8480,.T.);
#11191=ORIENTED_EDGE('',*,*,#8481,.F.);
#11192=ORIENTED_EDGE('',*,*,#8482,.F.);
#11193=ORIENTED_EDGE('',*,*,#8483,.T.);
#11194=ORIENTED_EDGE('',*,*,#8482,.T.);
#11195=ORIENTED_EDGE('',*,*,#8484,.F.);
#11196=ORIENTED_EDGE('',*,*,#8485,.F.);
#11197=ORIENTED_EDGE('',*,*,#8483,.F.);
#11198=ORIENTED_EDGE('',*,*,#8486,.F.);
#11199=ORIENTED_EDGE('',*,*,#8487,.F.);
#11200=ORIENTED_EDGE('',*,*,#8488,.F.);
#11201=ORIENTED_EDGE('',*,*,#8489,.F.);
#11202=ORIENTED_EDGE('',*,*,#8479,.F.);
#11203=ORIENTED_EDGE('',*,*,#8476,.T.);
#11204=ORIENTED_EDGE('',*,*,#8484,.T.);
#11205=ORIENTED_EDGE('',*,*,#8481,.T.);
#11206=ORIENTED_EDGE('',*,*,#8490,.T.);
#11207=ORIENTED_EDGE('',*,*,#8491,.T.);
#11208=ORIENTED_EDGE('',*,*,#8492,.T.);
#11209=ORIENTED_EDGE('',*,*,#8493,.T.);
#11210=ORIENTED_EDGE('',*,*,#8478,.F.);
#11211=ORIENTED_EDGE('',*,*,#8490,.F.);
#11212=ORIENTED_EDGE('',*,*,#8480,.F.);
#11213=ORIENTED_EDGE('',*,*,#8489,.T.);
#11214=ORIENTED_EDGE('',*,*,#8494,.T.);
#11215=ORIENTED_EDGE('',*,*,#8491,.F.);
#11216=ORIENTED_EDGE('',*,*,#8494,.F.);
#11217=ORIENTED_EDGE('',*,*,#8488,.T.);
#11218=ORIENTED_EDGE('',*,*,#8495,.T.);
#11219=ORIENTED_EDGE('',*,*,#8492,.F.);
#11220=ORIENTED_EDGE('',*,*,#8495,.F.);
#11221=ORIENTED_EDGE('',*,*,#8487,.T.);
#11222=ORIENTED_EDGE('',*,*,#8496,.T.);
#11223=ORIENTED_EDGE('',*,*,#8493,.F.);
#11224=ORIENTED_EDGE('',*,*,#8496,.F.);
#11225=ORIENTED_EDGE('',*,*,#8486,.T.);
#11226=ORIENTED_EDGE('',*,*,#8485,.T.);
#11227=ORIENTED_EDGE('',*,*,#8497,.T.);
#11228=ORIENTED_EDGE('',*,*,#8498,.T.);
#11229=ORIENTED_EDGE('',*,*,#8499,.F.);
#11230=ORIENTED_EDGE('',*,*,#8498,.F.);
#11231=ORIENTED_EDGE('',*,*,#8500,.T.);
#11232=ORIENTED_EDGE('',*,*,#8501,.T.);
#11233=ORIENTED_EDGE('',*,*,#8502,.T.);
#11234=ORIENTED_EDGE('',*,*,#8503,.F.);
#11235=ORIENTED_EDGE('',*,*,#8504,.F.);
#11236=ORIENTED_EDGE('',*,*,#8502,.F.);
#11237=ORIENTED_EDGE('',*,*,#8499,.T.);
#11238=ORIENTED_EDGE('',*,*,#8505,.T.);
#11239=ORIENTED_EDGE('',*,*,#8506,.F.);
#11240=ORIENTED_EDGE('',*,*,#8505,.F.);
#11241=ORIENTED_EDGE('',*,*,#8503,.T.);
#11242=ORIENTED_EDGE('',*,*,#8504,.T.);
#11243=ORIENTED_EDGE('',*,*,#8507,.T.);
#11244=ORIENTED_EDGE('',*,*,#8500,.F.);
#11245=ORIENTED_EDGE('',*,*,#8497,.F.);
#11246=ORIENTED_EDGE('',*,*,#8507,.F.);
#11247=ORIENTED_EDGE('',*,*,#8508,.T.);
#11248=ORIENTED_EDGE('',*,*,#8509,.T.);
#11249=ORIENTED_EDGE('',*,*,#8501,.F.);
#11250=ORIENTED_EDGE('',*,*,#8509,.F.);
#11251=ORIENTED_EDGE('',*,*,#8508,.F.);
#11252=ORIENTED_EDGE('',*,*,#8506,.T.);
#11253=ORIENTED_EDGE('',*,*,#8510,.F.);
#11254=ORIENTED_EDGE('',*,*,#8511,.T.);
#11255=ORIENTED_EDGE('',*,*,#8512,.T.);
#11256=ORIENTED_EDGE('',*,*,#8511,.F.);
#11257=ORIENTED_EDGE('',*,*,#8513,.F.);
#11258=ORIENTED_EDGE('',*,*,#8514,.T.);
#11259=ORIENTED_EDGE('',*,*,#8510,.T.);
#11260=ORIENTED_EDGE('',*,*,#8514,.F.);
#11261=ORIENTED_EDGE('',*,*,#8515,.F.);
#11262=ORIENTED_EDGE('',*,*,#8516,.F.);
#11263=ORIENTED_EDGE('',*,*,#8517,.F.);
#11264=ORIENTED_EDGE('',*,*,#8518,.T.);
#11265=ORIENTED_EDGE('',*,*,#8519,.F.);
#11266=ORIENTED_EDGE('',*,*,#8520,.F.);
#11267=ORIENTED_EDGE('',*,*,#8521,.F.);
#11268=ORIENTED_EDGE('',*,*,#8522,.F.);
#11269=ORIENTED_EDGE('',*,*,#8516,.T.);
#11270=ORIENTED_EDGE('',*,*,#8523,.F.);
#11271=ORIENTED_EDGE('',*,*,#8524,.F.);
#11272=ORIENTED_EDGE('',*,*,#8525,.F.);
#11273=ORIENTED_EDGE('',*,*,#8526,.F.);
#11274=ORIENTED_EDGE('',*,*,#8521,.T.);
#11275=ORIENTED_EDGE('',*,*,#8527,.F.);
#11276=ORIENTED_EDGE('',*,*,#8528,.F.);
#11277=ORIENTED_EDGE('',*,*,#8529,.F.);
#11278=ORIENTED_EDGE('',*,*,#8530,.F.);
#11279=ORIENTED_EDGE('',*,*,#8525,.T.);
#11280=ORIENTED_EDGE('',*,*,#8531,.F.);
#11281=ORIENTED_EDGE('',*,*,#8532,.F.);
#11282=ORIENTED_EDGE('',*,*,#8533,.F.);
#11283=ORIENTED_EDGE('',*,*,#8534,.F.);
#11284=ORIENTED_EDGE('',*,*,#8529,.T.);
#11285=ORIENTED_EDGE('',*,*,#8535,.F.);
#11286=ORIENTED_EDGE('',*,*,#8536,.F.);
#11287=ORIENTED_EDGE('',*,*,#8518,.F.);
#11288=ORIENTED_EDGE('',*,*,#8537,.F.);
#11289=ORIENTED_EDGE('',*,*,#8533,.T.);
#11290=ORIENTED_EDGE('',*,*,#8538,.F.);
#11291=ORIENTED_EDGE('',*,*,#8517,.T.);
#11292=ORIENTED_EDGE('',*,*,#8522,.T.);
#11293=ORIENTED_EDGE('',*,*,#8526,.T.);
#11294=ORIENTED_EDGE('',*,*,#8530,.T.);
#11295=ORIENTED_EDGE('',*,*,#8534,.T.);
#11296=ORIENTED_EDGE('',*,*,#8537,.T.);
#11297=ORIENTED_EDGE('',*,*,#8513,.T.);
#11298=ORIENTED_EDGE('',*,*,#8512,.F.);
#11299=ORIENTED_EDGE('',*,*,#8532,.T.);
#11300=ORIENTED_EDGE('',*,*,#8539,.T.);
#11301=ORIENTED_EDGE('',*,*,#8538,.T.);
#11302=ORIENTED_EDGE('',*,*,#8528,.T.);
#11303=ORIENTED_EDGE('',*,*,#8540,.T.);
#11304=ORIENTED_EDGE('',*,*,#8535,.T.);
#11305=ORIENTED_EDGE('',*,*,#8524,.T.);
#11306=ORIENTED_EDGE('',*,*,#8541,.T.);
#11307=ORIENTED_EDGE('',*,*,#8531,.T.);
#11308=ORIENTED_EDGE('',*,*,#8527,.T.);
#11309=ORIENTED_EDGE('',*,*,#8520,.T.);
#11310=ORIENTED_EDGE('',*,*,#8542,.F.);
#11311=ORIENTED_EDGE('',*,*,#8523,.T.);
#11312=ORIENTED_EDGE('',*,*,#8515,.T.);
#11313=ORIENTED_EDGE('',*,*,#8543,.T.);
#11314=ORIENTED_EDGE('',*,*,#8519,.T.);
#11315=ORIENTED_EDGE('',*,*,#8536,.T.);
#11316=ORIENTED_EDGE('',*,*,#8544,.T.);
#11317=ORIENTED_EDGE('',*,*,#8544,.F.);
#11318=ORIENTED_EDGE('',*,*,#8539,.F.);
#11319=ORIENTED_EDGE('',*,*,#8540,.F.);
#11320=ORIENTED_EDGE('',*,*,#8541,.F.);
#11321=ORIENTED_EDGE('',*,*,#8542,.T.);
#11322=ORIENTED_EDGE('',*,*,#8543,.F.);
#11323=ORIENTED_EDGE('',*,*,#8545,.F.);
#11324=ORIENTED_EDGE('',*,*,#8546,.T.);
#11325=ORIENTED_EDGE('',*,*,#8547,.T.);
#11326=ORIENTED_EDGE('',*,*,#8546,.F.);
#11327=ORIENTED_EDGE('',*,*,#8548,.F.);
#11328=ORIENTED_EDGE('',*,*,#8549,.T.);
#11329=ORIENTED_EDGE('',*,*,#8545,.T.);
#11330=ORIENTED_EDGE('',*,*,#8549,.F.);
#11331=ORIENTED_EDGE('',*,*,#8550,.F.);
#11332=ORIENTED_EDGE('',*,*,#8551,.F.);
#11333=ORIENTED_EDGE('',*,*,#8552,.F.);
#11334=ORIENTED_EDGE('',*,*,#8553,.T.);
#11335=ORIENTED_EDGE('',*,*,#8554,.F.);
#11336=ORIENTED_EDGE('',*,*,#8555,.F.);
#11337=ORIENTED_EDGE('',*,*,#8556,.F.);
#11338=ORIENTED_EDGE('',*,*,#8557,.F.);
#11339=ORIENTED_EDGE('',*,*,#8551,.T.);
#11340=ORIENTED_EDGE('',*,*,#8558,.F.);
#11341=ORIENTED_EDGE('',*,*,#8559,.F.);
#11342=ORIENTED_EDGE('',*,*,#8560,.F.);
#11343=ORIENTED_EDGE('',*,*,#8561,.F.);
#11344=ORIENTED_EDGE('',*,*,#8556,.T.);
#11345=ORIENTED_EDGE('',*,*,#8562,.F.);
#11346=ORIENTED_EDGE('',*,*,#8563,.F.);
#11347=ORIENTED_EDGE('',*,*,#8564,.F.);
#11348=ORIENTED_EDGE('',*,*,#8565,.F.);
#11349=ORIENTED_EDGE('',*,*,#8560,.T.);
#11350=ORIENTED_EDGE('',*,*,#8566,.F.);
#11351=ORIENTED_EDGE('',*,*,#8567,.F.);
#11352=ORIENTED_EDGE('',*,*,#8568,.F.);
#11353=ORIENTED_EDGE('',*,*,#8569,.F.);
#11354=ORIENTED_EDGE('',*,*,#8564,.T.);
#11355=ORIENTED_EDGE('',*,*,#8570,.F.);
#11356=ORIENTED_EDGE('',*,*,#8571,.F.);
#11357=ORIENTED_EDGE('',*,*,#8553,.F.);
#11358=ORIENTED_EDGE('',*,*,#8572,.F.);
#11359=ORIENTED_EDGE('',*,*,#8568,.T.);
#11360=ORIENTED_EDGE('',*,*,#8573,.F.);
#11361=ORIENTED_EDGE('',*,*,#8552,.T.);
#11362=ORIENTED_EDGE('',*,*,#8557,.T.);
#11363=ORIENTED_EDGE('',*,*,#8561,.T.);
#11364=ORIENTED_EDGE('',*,*,#8565,.T.);
#11365=ORIENTED_EDGE('',*,*,#8569,.T.);
#11366=ORIENTED_EDGE('',*,*,#8572,.T.);
#11367=ORIENTED_EDGE('',*,*,#8548,.T.);
#11368=ORIENTED_EDGE('',*,*,#8547,.F.);
#11369=ORIENTED_EDGE('',*,*,#8567,.T.);
#11370=ORIENTED_EDGE('',*,*,#8574,.T.);
#11371=ORIENTED_EDGE('',*,*,#8573,.T.);
#11372=ORIENTED_EDGE('',*,*,#8563,.T.);
#11373=ORIENTED_EDGE('',*,*,#8575,.T.);
#11374=ORIENTED_EDGE('',*,*,#8570,.T.);
#11375=ORIENTED_EDGE('',*,*,#8559,.T.);
#11376=ORIENTED_EDGE('',*,*,#8576,.T.);
#11377=ORIENTED_EDGE('',*,*,#8566,.T.);
#11378=ORIENTED_EDGE('',*,*,#8562,.T.);
#11379=ORIENTED_EDGE('',*,*,#8555,.T.);
#11380=ORIENTED_EDGE('',*,*,#8577,.F.);
#11381=ORIENTED_EDGE('',*,*,#8558,.T.);
#11382=ORIENTED_EDGE('',*,*,#8550,.T.);
#11383=ORIENTED_EDGE('',*,*,#8578,.T.);
#11384=ORIENTED_EDGE('',*,*,#8554,.T.);
#11385=ORIENTED_EDGE('',*,*,#8571,.T.);
#11386=ORIENTED_EDGE('',*,*,#8579,.T.);
#11387=ORIENTED_EDGE('',*,*,#8579,.F.);
#11388=ORIENTED_EDGE('',*,*,#8574,.F.);
#11389=ORIENTED_EDGE('',*,*,#8575,.F.);
#11390=ORIENTED_EDGE('',*,*,#8576,.F.);
#11391=ORIENTED_EDGE('',*,*,#8577,.T.);
#11392=ORIENTED_EDGE('',*,*,#8578,.F.);
#11393=ORIENTED_EDGE('',*,*,#8580,.F.);
#11394=ORIENTED_EDGE('',*,*,#8581,.T.);
#11395=ORIENTED_EDGE('',*,*,#8582,.T.);
#11396=ORIENTED_EDGE('',*,*,#8583,.T.);
#11397=ORIENTED_EDGE('',*,*,#8581,.F.);
#11398=ORIENTED_EDGE('',*,*,#8584,.T.);
#11399=ORIENTED_EDGE('',*,*,#8585,.T.);
#11400=ORIENTED_EDGE('',*,*,#8582,.F.);
#11401=ORIENTED_EDGE('',*,*,#8583,.F.);
#11402=ORIENTED_EDGE('',*,*,#8585,.F.);
#11403=ORIENTED_EDGE('',*,*,#8586,.T.);
#11404=ORIENTED_EDGE('',*,*,#8587,.T.);
#11405=ORIENTED_EDGE('',*,*,#8588,.T.);
#11406=ORIENTED_EDGE('',*,*,#8589,.T.);
#11407=ORIENTED_EDGE('',*,*,#8588,.F.);
#11408=ORIENTED_EDGE('',*,*,#8584,.F.);
#11409=ORIENTED_EDGE('',*,*,#8590,.T.);
#11410=ORIENTED_EDGE('',*,*,#8587,.F.);
#11411=ORIENTED_EDGE('',*,*,#8590,.F.);
#11412=ORIENTED_EDGE('',*,*,#8586,.F.);
#11413=ORIENTED_EDGE('',*,*,#8591,.T.);
#11414=ORIENTED_EDGE('',*,*,#8592,.T.);
#11415=ORIENTED_EDGE('',*,*,#8593,.T.);
#11416=ORIENTED_EDGE('',*,*,#8594,.F.);
#11417=ORIENTED_EDGE('',*,*,#8595,.F.);
#11418=ORIENTED_EDGE('',*,*,#8596,.F.);
#11419=ORIENTED_EDGE('',*,*,#8594,.T.);
#11420=ORIENTED_EDGE('',*,*,#8597,.T.);
#11421=ORIENTED_EDGE('',*,*,#8598,.T.);
#11422=ORIENTED_EDGE('',*,*,#8599,.F.);
#11423=ORIENTED_EDGE('',*,*,#8600,.F.);
#11424=ORIENTED_EDGE('',*,*,#8601,.F.);
#11425=ORIENTED_EDGE('',*,*,#8602,.F.);
#11426=ORIENTED_EDGE('',*,*,#8603,.F.);
#11427=ORIENTED_EDGE('',*,*,#8604,.T.);
#11428=ORIENTED_EDGE('',*,*,#8605,.T.);
#11429=ORIENTED_EDGE('',*,*,#8599,.T.);
#11430=ORIENTED_EDGE('',*,*,#8606,.F.);
#11431=ORIENTED_EDGE('',*,*,#8603,.T.);
#11432=ORIENTED_EDGE('',*,*,#8607,.T.);
#11433=ORIENTED_EDGE('',*,*,#8608,.T.);
#11434=ORIENTED_EDGE('',*,*,#8609,.F.);
#11435=ORIENTED_EDGE('',*,*,#8610,.F.);
#11436=ORIENTED_EDGE('',*,*,#8611,.F.);
#11437=ORIENTED_EDGE('',*,*,#8609,.T.);
#11438=ORIENTED_EDGE('',*,*,#8612,.T.);
#11439=ORIENTED_EDGE('',*,*,#8613,.T.);
#11440=ORIENTED_EDGE('',*,*,#8614,.F.);
#11441=ORIENTED_EDGE('',*,*,#8615,.F.);
#11442=ORIENTED_EDGE('',*,*,#8616,.F.);
#11443=ORIENTED_EDGE('',*,*,#8614,.T.);
#11444=ORIENTED_EDGE('',*,*,#8617,.T.);
#11445=ORIENTED_EDGE('',*,*,#8618,.T.);
#11446=ORIENTED_EDGE('',*,*,#8591,.F.);
#11447=ORIENTED_EDGE('',*,*,#8619,.F.);
#11448=ORIENTED_EDGE('',*,*,#8620,.F.);
#11449=ORIENTED_EDGE('',*,*,#8621,.F.);
#11450=ORIENTED_EDGE('',*,*,#8622,.F.);
#11451=ORIENTED_EDGE('',*,*,#8623,.F.);
#11452=ORIENTED_EDGE('',*,*,#8624,.F.);
#11453=ORIENTED_EDGE('',*,*,#8625,.T.);
#11454=ORIENTED_EDGE('',*,*,#8626,.F.);
#11455=ORIENTED_EDGE('',*,*,#8589,.F.);
#11456=ORIENTED_EDGE('',*,*,#8627,.F.);
#11457=ORIENTED_EDGE('',*,*,#8628,.F.);
#11458=ORIENTED_EDGE('',*,*,#8629,.F.);
#11459=ORIENTED_EDGE('',*,*,#8630,.F.);
#11460=ORIENTED_EDGE('',*,*,#8631,.F.);
#11461=ORIENTED_EDGE('',*,*,#8632,.F.);
#11462=ORIENTED_EDGE('',*,*,#8580,.T.);
#11463=ORIENTED_EDGE('',*,*,#8596,.T.);
#11464=ORIENTED_EDGE('',*,*,#8628,.T.);
#11465=ORIENTED_EDGE('',*,*,#8619,.T.);
#11466=ORIENTED_EDGE('',*,*,#8595,.T.);
#11467=ORIENTED_EDGE('',*,*,#8601,.T.);
#11468=ORIENTED_EDGE('',*,*,#8629,.T.);
#11469=ORIENTED_EDGE('',*,*,#8600,.T.);
#11470=ORIENTED_EDGE('',*,*,#8605,.F.);
#11471=ORIENTED_EDGE('',*,*,#8630,.T.);
#11472=ORIENTED_EDGE('',*,*,#8611,.T.);
#11473=ORIENTED_EDGE('',*,*,#8631,.T.);
#11474=ORIENTED_EDGE('',*,*,#8604,.F.);
#11475=ORIENTED_EDGE('',*,*,#8610,.T.);
#11476=ORIENTED_EDGE('',*,*,#8616,.T.);
#11477=ORIENTED_EDGE('',*,*,#8632,.T.);
#11478=ORIENTED_EDGE('',*,*,#8615,.T.);
#11479=ORIENTED_EDGE('',*,*,#8620,.T.);
#11480=ORIENTED_EDGE('',*,*,#8627,.T.);
#11481=ORIENTED_EDGE('',*,*,#8622,.T.);
#11482=ORIENTED_EDGE('',*,*,#8617,.F.);
#11483=ORIENTED_EDGE('',*,*,#8613,.F.);
#11484=ORIENTED_EDGE('',*,*,#8623,.T.);
#11485=ORIENTED_EDGE('',*,*,#8612,.F.);
#11486=ORIENTED_EDGE('',*,*,#8608,.F.);
#11487=ORIENTED_EDGE('',*,*,#8602,.T.);
#11488=ORIENTED_EDGE('',*,*,#8624,.T.);
#11489=ORIENTED_EDGE('',*,*,#8607,.F.);
#11490=ORIENTED_EDGE('',*,*,#8625,.F.);
#11491=ORIENTED_EDGE('',*,*,#8606,.T.);
#11492=ORIENTED_EDGE('',*,*,#8598,.F.);
#11493=ORIENTED_EDGE('',*,*,#8626,.T.);
#11494=ORIENTED_EDGE('',*,*,#8597,.F.);
#11495=ORIENTED_EDGE('',*,*,#8593,.F.);
#11496=ORIENTED_EDGE('',*,*,#8618,.F.);
#11497=ORIENTED_EDGE('',*,*,#8621,.T.);
#11498=ORIENTED_EDGE('',*,*,#8592,.F.);
#11499=ORIENTED_EDGE('',*,*,#8633,.F.);
#11500=ORIENTED_EDGE('',*,*,#8634,.F.);
#11501=ORIENTED_EDGE('',*,*,#8635,.F.);
#11502=ORIENTED_EDGE('',*,*,#8636,.T.);
#11503=ORIENTED_EDGE('',*,*,#8637,.F.);
#11504=ORIENTED_EDGE('',*,*,#8638,.F.);
#11505=ORIENTED_EDGE('',*,*,#8633,.T.);
#11506=ORIENTED_EDGE('',*,*,#8639,.T.);
#11507=ORIENTED_EDGE('',*,*,#8640,.F.);
#11508=ORIENTED_EDGE('',*,*,#8641,.F.);
#11509=ORIENTED_EDGE('',*,*,#8637,.T.);
#11510=ORIENTED_EDGE('',*,*,#8642,.T.);
#11511=ORIENTED_EDGE('',*,*,#8643,.F.);
#11512=ORIENTED_EDGE('',*,*,#8644,.F.);
#11513=ORIENTED_EDGE('',*,*,#8640,.T.);
#11514=ORIENTED_EDGE('',*,*,#8645,.T.);
#11515=ORIENTED_EDGE('',*,*,#8646,.F.);
#11516=ORIENTED_EDGE('',*,*,#8647,.F.);
#11517=ORIENTED_EDGE('',*,*,#8643,.T.);
#11518=ORIENTED_EDGE('',*,*,#8648,.T.);
#11519=ORIENTED_EDGE('',*,*,#8649,.F.);
#11520=ORIENTED_EDGE('',*,*,#8650,.F.);
#11521=ORIENTED_EDGE('',*,*,#8646,.T.);
#11522=ORIENTED_EDGE('',*,*,#8651,.T.);
#11523=ORIENTED_EDGE('',*,*,#8652,.F.);
#11524=ORIENTED_EDGE('',*,*,#8653,.F.);
#11525=ORIENTED_EDGE('',*,*,#8649,.T.);
#11526=ORIENTED_EDGE('',*,*,#8654,.T.);
#11527=ORIENTED_EDGE('',*,*,#8655,.F.);
#11528=ORIENTED_EDGE('',*,*,#8656,.F.);
#11529=ORIENTED_EDGE('',*,*,#8652,.T.);
#11530=ORIENTED_EDGE('',*,*,#8657,.T.);
#11531=ORIENTED_EDGE('',*,*,#8658,.F.);
#11532=ORIENTED_EDGE('',*,*,#8659,.F.);
#11533=ORIENTED_EDGE('',*,*,#8655,.T.);
#11534=ORIENTED_EDGE('',*,*,#8660,.T.);
#11535=ORIENTED_EDGE('',*,*,#8661,.F.);
#11536=ORIENTED_EDGE('',*,*,#8662,.F.);
#11537=ORIENTED_EDGE('',*,*,#8658,.T.);
#11538=ORIENTED_EDGE('',*,*,#8663,.T.);
#11539=ORIENTED_EDGE('',*,*,#8664,.F.);
#11540=ORIENTED_EDGE('',*,*,#8665,.F.);
#11541=ORIENTED_EDGE('',*,*,#8661,.T.);
#11542=ORIENTED_EDGE('',*,*,#8666,.T.);
#11543=ORIENTED_EDGE('',*,*,#8667,.F.);
#11544=ORIENTED_EDGE('',*,*,#8668,.F.);
#11545=ORIENTED_EDGE('',*,*,#8664,.T.);
#11546=ORIENTED_EDGE('',*,*,#8669,.T.);
#11547=ORIENTED_EDGE('',*,*,#8670,.F.);
#11548=ORIENTED_EDGE('',*,*,#8671,.F.);
#11549=ORIENTED_EDGE('',*,*,#8667,.T.);
#11550=ORIENTED_EDGE('',*,*,#8672,.T.);
#11551=ORIENTED_EDGE('',*,*,#8673,.F.);
#11552=ORIENTED_EDGE('',*,*,#8674,.F.);
#11553=ORIENTED_EDGE('',*,*,#8670,.T.);
#11554=ORIENTED_EDGE('',*,*,#8675,.T.);
#11555=ORIENTED_EDGE('',*,*,#8676,.F.);
#11556=ORIENTED_EDGE('',*,*,#8677,.F.);
#11557=ORIENTED_EDGE('',*,*,#8673,.T.);
#11558=ORIENTED_EDGE('',*,*,#8678,.T.);
#11559=ORIENTED_EDGE('',*,*,#8679,.F.);
#11560=ORIENTED_EDGE('',*,*,#8680,.F.);
#11561=ORIENTED_EDGE('',*,*,#8676,.T.);
#11562=ORIENTED_EDGE('',*,*,#8681,.T.);
#11563=ORIENTED_EDGE('',*,*,#8682,.F.);
#11564=ORIENTED_EDGE('',*,*,#8683,.F.);
#11565=ORIENTED_EDGE('',*,*,#8679,.T.);
#11566=ORIENTED_EDGE('',*,*,#8684,.T.);
#11567=ORIENTED_EDGE('',*,*,#8685,.F.);
#11568=ORIENTED_EDGE('',*,*,#8686,.F.);
#11569=ORIENTED_EDGE('',*,*,#8682,.T.);
#11570=ORIENTED_EDGE('',*,*,#8687,.T.);
#11571=ORIENTED_EDGE('',*,*,#8688,.F.);
#11572=ORIENTED_EDGE('',*,*,#8689,.F.);
#11573=ORIENTED_EDGE('',*,*,#8685,.T.);
#11574=ORIENTED_EDGE('',*,*,#8690,.T.);
#11575=ORIENTED_EDGE('',*,*,#8691,.F.);
#11576=ORIENTED_EDGE('',*,*,#8692,.F.);
#11577=ORIENTED_EDGE('',*,*,#8688,.T.);
#11578=ORIENTED_EDGE('',*,*,#8693,.T.);
#11579=ORIENTED_EDGE('',*,*,#8694,.F.);
#11580=ORIENTED_EDGE('',*,*,#8695,.F.);
#11581=ORIENTED_EDGE('',*,*,#8691,.T.);
#11582=ORIENTED_EDGE('',*,*,#8696,.T.);
#11583=ORIENTED_EDGE('',*,*,#8697,.F.);
#11584=ORIENTED_EDGE('',*,*,#8698,.F.);
#11585=ORIENTED_EDGE('',*,*,#8694,.T.);
#11586=ORIENTED_EDGE('',*,*,#8699,.T.);
#11587=ORIENTED_EDGE('',*,*,#8700,.F.);
#11588=ORIENTED_EDGE('',*,*,#8701,.T.);
#11589=ORIENTED_EDGE('',*,*,#8702,.T.);
#11590=ORIENTED_EDGE('',*,*,#8703,.T.);
#11591=ORIENTED_EDGE('',*,*,#8704,.T.);
#11592=ORIENTED_EDGE('',*,*,#8705,.T.);
#11593=ORIENTED_EDGE('',*,*,#8706,.T.);
#11594=ORIENTED_EDGE('',*,*,#8707,.T.);
#11595=ORIENTED_EDGE('',*,*,#8708,.T.);
#11596=ORIENTED_EDGE('',*,*,#8702,.F.);
#11597=ORIENTED_EDGE('',*,*,#8709,.T.);
#11598=ORIENTED_EDGE('',*,*,#8710,.T.);
#11599=ORIENTED_EDGE('',*,*,#8711,.F.);
#11600=ORIENTED_EDGE('',*,*,#8712,.F.);
#11601=ORIENTED_EDGE('',*,*,#8713,.T.);
#11602=ORIENTED_EDGE('',*,*,#8700,.T.);
#11603=ORIENTED_EDGE('',*,*,#8714,.F.);
#11604=ORIENTED_EDGE('',*,*,#8715,.F.);
#11605=ORIENTED_EDGE('',*,*,#8716,.T.);
#11606=ORIENTED_EDGE('',*,*,#8712,.T.);
#11607=ORIENTED_EDGE('',*,*,#8717,.F.);
#11608=ORIENTED_EDGE('',*,*,#8718,.F.);
#11609=ORIENTED_EDGE('',*,*,#8719,.T.);
#11610=ORIENTED_EDGE('',*,*,#8715,.T.);
#11611=ORIENTED_EDGE('',*,*,#8720,.F.);
#11612=ORIENTED_EDGE('',*,*,#8721,.F.);
#11613=ORIENTED_EDGE('',*,*,#8722,.T.);
#11614=ORIENTED_EDGE('',*,*,#8718,.T.);
#11615=ORIENTED_EDGE('',*,*,#8723,.F.);
#11616=ORIENTED_EDGE('',*,*,#8724,.F.);
#11617=ORIENTED_EDGE('',*,*,#8725,.T.);
#11618=ORIENTED_EDGE('',*,*,#8721,.T.);
#11619=ORIENTED_EDGE('',*,*,#8726,.F.);
#11620=ORIENTED_EDGE('',*,*,#8727,.F.);
#11621=ORIENTED_EDGE('',*,*,#8728,.T.);
#11622=ORIENTED_EDGE('',*,*,#8724,.T.);
#11623=ORIENTED_EDGE('',*,*,#8729,.F.);
#11624=ORIENTED_EDGE('',*,*,#8730,.F.);
#11625=ORIENTED_EDGE('',*,*,#8731,.T.);
#11626=ORIENTED_EDGE('',*,*,#8727,.T.);
#11627=ORIENTED_EDGE('',*,*,#8732,.F.);
#11628=ORIENTED_EDGE('',*,*,#8733,.F.);
#11629=ORIENTED_EDGE('',*,*,#8734,.T.);
#11630=ORIENTED_EDGE('',*,*,#8730,.T.);
#11631=ORIENTED_EDGE('',*,*,#8735,.F.);
#11632=ORIENTED_EDGE('',*,*,#8736,.F.);
#11633=ORIENTED_EDGE('',*,*,#8737,.T.);
#11634=ORIENTED_EDGE('',*,*,#8733,.T.);
#11635=ORIENTED_EDGE('',*,*,#8738,.F.);
#11636=ORIENTED_EDGE('',*,*,#8739,.F.);
#11637=ORIENTED_EDGE('',*,*,#8740,.T.);
#11638=ORIENTED_EDGE('',*,*,#8736,.T.);
#11639=ORIENTED_EDGE('',*,*,#8741,.F.);
#11640=ORIENTED_EDGE('',*,*,#8742,.F.);
#11641=ORIENTED_EDGE('',*,*,#8743,.T.);
#11642=ORIENTED_EDGE('',*,*,#8739,.T.);
#11643=ORIENTED_EDGE('',*,*,#8744,.F.);
#11644=ORIENTED_EDGE('',*,*,#8745,.F.);
#11645=ORIENTED_EDGE('',*,*,#8746,.T.);
#11646=ORIENTED_EDGE('',*,*,#8742,.T.);
#11647=ORIENTED_EDGE('',*,*,#8747,.F.);
#11648=ORIENTED_EDGE('',*,*,#8748,.F.);
#11649=ORIENTED_EDGE('',*,*,#8749,.T.);
#11650=ORIENTED_EDGE('',*,*,#8745,.T.);
#11651=ORIENTED_EDGE('',*,*,#8750,.F.);
#11652=ORIENTED_EDGE('',*,*,#8751,.F.);
#11653=ORIENTED_EDGE('',*,*,#8752,.T.);
#11654=ORIENTED_EDGE('',*,*,#8748,.T.);
#11655=ORIENTED_EDGE('',*,*,#8753,.F.);
#11656=ORIENTED_EDGE('',*,*,#8754,.F.);
#11657=ORIENTED_EDGE('',*,*,#8755,.T.);
#11658=ORIENTED_EDGE('',*,*,#8751,.T.);
#11659=ORIENTED_EDGE('',*,*,#8756,.F.);
#11660=ORIENTED_EDGE('',*,*,#8757,.F.);
#11661=ORIENTED_EDGE('',*,*,#8758,.T.);
#11662=ORIENTED_EDGE('',*,*,#8754,.T.);
#11663=ORIENTED_EDGE('',*,*,#8759,.F.);
#11664=ORIENTED_EDGE('',*,*,#8760,.F.);
#11665=ORIENTED_EDGE('',*,*,#8761,.T.);
#11666=ORIENTED_EDGE('',*,*,#8757,.T.);
#11667=ORIENTED_EDGE('',*,*,#8762,.F.);
#11668=ORIENTED_EDGE('',*,*,#8763,.F.);
#11669=ORIENTED_EDGE('',*,*,#8764,.T.);
#11670=ORIENTED_EDGE('',*,*,#8760,.T.);
#11671=ORIENTED_EDGE('',*,*,#8765,.F.);
#11672=ORIENTED_EDGE('',*,*,#8766,.F.);
#11673=ORIENTED_EDGE('',*,*,#8767,.T.);
#11674=ORIENTED_EDGE('',*,*,#8763,.T.);
#11675=ORIENTED_EDGE('',*,*,#8768,.F.);
#11676=ORIENTED_EDGE('',*,*,#8769,.F.);
#11677=ORIENTED_EDGE('',*,*,#8770,.T.);
#11678=ORIENTED_EDGE('',*,*,#8771,.T.);
#11679=ORIENTED_EDGE('',*,*,#8766,.T.);
#11680=ORIENTED_EDGE('',*,*,#8772,.F.);
#11681=ORIENTED_EDGE('',*,*,#8773,.F.);
#11682=ORIENTED_EDGE('',*,*,#8774,.T.);
#11683=ORIENTED_EDGE('',*,*,#8775,.F.);
#11684=ORIENTED_EDGE('',*,*,#8776,.F.);
#11685=ORIENTED_EDGE('',*,*,#8777,.F.);
#11686=ORIENTED_EDGE('',*,*,#8778,.T.);
#11687=ORIENTED_EDGE('',*,*,#8779,.F.);
#11688=ORIENTED_EDGE('',*,*,#8780,.F.);
#11689=ORIENTED_EDGE('',*,*,#8781,.F.);
#11690=ORIENTED_EDGE('',*,*,#8782,.T.);
#11691=ORIENTED_EDGE('',*,*,#8783,.T.);
#11692=ORIENTED_EDGE('',*,*,#8782,.F.);
#11693=ORIENTED_EDGE('',*,*,#8779,.T.);
#11694=ORIENTED_EDGE('',*,*,#8784,.T.);
#11695=ORIENTED_EDGE('',*,*,#8773,.T.);
#11696=ORIENTED_EDGE('',*,*,#8785,.T.);
#11697=ORIENTED_EDGE('',*,*,#8635,.T.);
#11698=ORIENTED_EDGE('',*,*,#8786,.T.);
#11699=ORIENTED_EDGE('',*,*,#8770,.F.);
#11700=ORIENTED_EDGE('',*,*,#8787,.F.);
#11701=ORIENTED_EDGE('',*,*,#8788,.T.);
#11702=ORIENTED_EDGE('',*,*,#8789,.T.);
#11703=ORIENTED_EDGE('',*,*,#8790,.F.);
#11704=ORIENTED_EDGE('',*,*,#8789,.F.);
#11705=ORIENTED_EDGE('',*,*,#8791,.T.);
#11706=ORIENTED_EDGE('',*,*,#8769,.T.);
#11707=ORIENTED_EDGE('',*,*,#8792,.F.);
#11708=ORIENTED_EDGE('',*,*,#8787,.T.);
#11709=ORIENTED_EDGE('',*,*,#8777,.T.);
#11710=ORIENTED_EDGE('',*,*,#8793,.T.);
#11711=ORIENTED_EDGE('',*,*,#8794,.T.);
#11712=ORIENTED_EDGE('',*,*,#8795,.T.);
#11713=ORIENTED_EDGE('',*,*,#8796,.T.);
#11714=ORIENTED_EDGE('',*,*,#8781,.T.);
#11715=ORIENTED_EDGE('',*,*,#8797,.T.);
#11716=ORIENTED_EDGE('',*,*,#8798,.T.);
#11717=ORIENTED_EDGE('',*,*,#8799,.T.);
#11718=ORIENTED_EDGE('',*,*,#8800,.T.);
#11719=ORIENTED_EDGE('',*,*,#8775,.T.);
#11720=ORIENTED_EDGE('',*,*,#8783,.F.);
#11721=ORIENTED_EDGE('',*,*,#8790,.T.);
#11722=ORIENTED_EDGE('',*,*,#8801,.F.);
#11723=ORIENTED_EDGE('',*,*,#8710,.F.);
#11724=ORIENTED_EDGE('',*,*,#8802,.F.);
#11725=ORIENTED_EDGE('',*,*,#8803,.F.);
#11726=ORIENTED_EDGE('',*,*,#8792,.T.);
#11727=ORIENTED_EDGE('',*,*,#8772,.T.);
#11728=ORIENTED_EDGE('',*,*,#8768,.T.);
#11729=ORIENTED_EDGE('',*,*,#8765,.T.);
#11730=ORIENTED_EDGE('',*,*,#8762,.T.);
#11731=ORIENTED_EDGE('',*,*,#8759,.T.);
#11732=ORIENTED_EDGE('',*,*,#8756,.T.);
#11733=ORIENTED_EDGE('',*,*,#8753,.T.);
#11734=ORIENTED_EDGE('',*,*,#8750,.T.);
#11735=ORIENTED_EDGE('',*,*,#8747,.T.);
#11736=ORIENTED_EDGE('',*,*,#8744,.T.);
#11737=ORIENTED_EDGE('',*,*,#8741,.T.);
#11738=ORIENTED_EDGE('',*,*,#8738,.T.);
#11739=ORIENTED_EDGE('',*,*,#8735,.T.);
#11740=ORIENTED_EDGE('',*,*,#8732,.T.);
#11741=ORIENTED_EDGE('',*,*,#8729,.T.);
#11742=ORIENTED_EDGE('',*,*,#8726,.T.);
#11743=ORIENTED_EDGE('',*,*,#8723,.T.);
#11744=ORIENTED_EDGE('',*,*,#8720,.T.);
#11745=ORIENTED_EDGE('',*,*,#8717,.T.);
#11746=ORIENTED_EDGE('',*,*,#8714,.T.);
#11747=ORIENTED_EDGE('',*,*,#8711,.T.);
#11748=ORIENTED_EDGE('',*,*,#8801,.T.);
#11749=ORIENTED_EDGE('',*,*,#8804,.F.);
#11750=ORIENTED_EDGE('',*,*,#8699,.F.);
#11751=ORIENTED_EDGE('',*,*,#8696,.F.);
#11752=ORIENTED_EDGE('',*,*,#8693,.F.);
#11753=ORIENTED_EDGE('',*,*,#8690,.F.);
#11754=ORIENTED_EDGE('',*,*,#8687,.F.);
#11755=ORIENTED_EDGE('',*,*,#8684,.F.);
#11756=ORIENTED_EDGE('',*,*,#8681,.F.);
#11757=ORIENTED_EDGE('',*,*,#8678,.F.);
#11758=ORIENTED_EDGE('',*,*,#8675,.F.);
#11759=ORIENTED_EDGE('',*,*,#8672,.F.);
#11760=ORIENTED_EDGE('',*,*,#8669,.F.);
#11761=ORIENTED_EDGE('',*,*,#8666,.F.);
#11762=ORIENTED_EDGE('',*,*,#8663,.F.);
#11763=ORIENTED_EDGE('',*,*,#8660,.F.);
#11764=ORIENTED_EDGE('',*,*,#8657,.F.);
#11765=ORIENTED_EDGE('',*,*,#8654,.F.);
#11766=ORIENTED_EDGE('',*,*,#8651,.F.);
#11767=ORIENTED_EDGE('',*,*,#8648,.F.);
#11768=ORIENTED_EDGE('',*,*,#8645,.F.);
#11769=ORIENTED_EDGE('',*,*,#8642,.F.);
#11770=ORIENTED_EDGE('',*,*,#8639,.F.);
#11771=ORIENTED_EDGE('',*,*,#8636,.F.);
#11772=ORIENTED_EDGE('',*,*,#8791,.F.);
#11773=ORIENTED_EDGE('',*,*,#8788,.F.);
#11774=ORIENTED_EDGE('',*,*,#8697,.T.);
#11775=ORIENTED_EDGE('',*,*,#8804,.T.);
#11776=ORIENTED_EDGE('',*,*,#8803,.T.);
#11777=ORIENTED_EDGE('',*,*,#8805,.F.);
#11778=ORIENTED_EDGE('',*,*,#8634,.T.);
#11779=ORIENTED_EDGE('',*,*,#8638,.T.);
#11780=ORIENTED_EDGE('',*,*,#8641,.T.);
#11781=ORIENTED_EDGE('',*,*,#8644,.T.);
#11782=ORIENTED_EDGE('',*,*,#8647,.T.);
#11783=ORIENTED_EDGE('',*,*,#8650,.T.);
#11784=ORIENTED_EDGE('',*,*,#8653,.T.);
#11785=ORIENTED_EDGE('',*,*,#8656,.T.);
#11786=ORIENTED_EDGE('',*,*,#8659,.T.);
#11787=ORIENTED_EDGE('',*,*,#8662,.T.);
#11788=ORIENTED_EDGE('',*,*,#8665,.T.);
#11789=ORIENTED_EDGE('',*,*,#8668,.T.);
#11790=ORIENTED_EDGE('',*,*,#8671,.T.);
#11791=ORIENTED_EDGE('',*,*,#8674,.T.);
#11792=ORIENTED_EDGE('',*,*,#8677,.T.);
#11793=ORIENTED_EDGE('',*,*,#8680,.T.);
#11794=ORIENTED_EDGE('',*,*,#8683,.T.);
#11795=ORIENTED_EDGE('',*,*,#8686,.T.);
#11796=ORIENTED_EDGE('',*,*,#8689,.T.);
#11797=ORIENTED_EDGE('',*,*,#8692,.T.);
#11798=ORIENTED_EDGE('',*,*,#8695,.T.);
#11799=ORIENTED_EDGE('',*,*,#8698,.T.);
#11800=ORIENTED_EDGE('',*,*,#8805,.T.);
#11801=ORIENTED_EDGE('',*,*,#8802,.T.);
#11802=ORIENTED_EDGE('',*,*,#8709,.F.);
#11803=ORIENTED_EDGE('',*,*,#8701,.F.);
#11804=ORIENTED_EDGE('',*,*,#8713,.F.);
#11805=ORIENTED_EDGE('',*,*,#8716,.F.);
#11806=ORIENTED_EDGE('',*,*,#8719,.F.);
#11807=ORIENTED_EDGE('',*,*,#8722,.F.);
#11808=ORIENTED_EDGE('',*,*,#8725,.F.);
#11809=ORIENTED_EDGE('',*,*,#8728,.F.);
#11810=ORIENTED_EDGE('',*,*,#8731,.F.);
#11811=ORIENTED_EDGE('',*,*,#8734,.F.);
#11812=ORIENTED_EDGE('',*,*,#8737,.F.);
#11813=ORIENTED_EDGE('',*,*,#8740,.F.);
#11814=ORIENTED_EDGE('',*,*,#8743,.F.);
#11815=ORIENTED_EDGE('',*,*,#8746,.F.);
#11816=ORIENTED_EDGE('',*,*,#8749,.F.);
#11817=ORIENTED_EDGE('',*,*,#8752,.F.);
#11818=ORIENTED_EDGE('',*,*,#8755,.F.);
#11819=ORIENTED_EDGE('',*,*,#8758,.F.);
#11820=ORIENTED_EDGE('',*,*,#8761,.F.);
#11821=ORIENTED_EDGE('',*,*,#8764,.F.);
#11822=ORIENTED_EDGE('',*,*,#8767,.F.);
#11823=ORIENTED_EDGE('',*,*,#8771,.F.);
#11824=ORIENTED_EDGE('',*,*,#8786,.F.);
#11825=ORIENTED_EDGE('',*,*,#8703,.F.);
#11826=ORIENTED_EDGE('',*,*,#8806,.T.);
#11827=ORIENTED_EDGE('',*,*,#8807,.F.);
#11828=ORIENTED_EDGE('',*,*,#8807,.T.);
#11829=ORIENTED_EDGE('',*,*,#8808,.T.);
#11830=ORIENTED_EDGE('',*,*,#8785,.F.);
#11831=ORIENTED_EDGE('',*,*,#8809,.T.);
#11832=ORIENTED_EDGE('',*,*,#8810,.F.);
#11833=ORIENTED_EDGE('',*,*,#8704,.F.);
#11834=ORIENTED_EDGE('',*,*,#8810,.T.);
#11835=ORIENTED_EDGE('',*,*,#8811,.T.);
#11836=ORIENTED_EDGE('',*,*,#8705,.F.);
#11837=ORIENTED_EDGE('',*,*,#8706,.F.);
#11838=ORIENTED_EDGE('',*,*,#8812,.T.);
#11839=ORIENTED_EDGE('',*,*,#8813,.F.);
#11840=ORIENTED_EDGE('',*,*,#8813,.T.);
#11841=ORIENTED_EDGE('',*,*,#8814,.T.);
#11842=ORIENTED_EDGE('',*,*,#8784,.F.);
#11843=ORIENTED_EDGE('',*,*,#8815,.T.);
#11844=ORIENTED_EDGE('',*,*,#8816,.F.);
#11845=ORIENTED_EDGE('',*,*,#8707,.F.);
#11846=ORIENTED_EDGE('',*,*,#8816,.T.);
#11847=ORIENTED_EDGE('',*,*,#8817,.T.);
#11848=ORIENTED_EDGE('',*,*,#8708,.F.);
#11849=ORIENTED_EDGE('',*,*,#8795,.F.);
#11850=ORIENTED_EDGE('',*,*,#8817,.F.);
#11851=ORIENTED_EDGE('',*,*,#8818,.F.);
#11852=ORIENTED_EDGE('',*,*,#8818,.T.);
#11853=ORIENTED_EDGE('',*,*,#8815,.F.);
#11854=ORIENTED_EDGE('',*,*,#8778,.F.);
#11855=ORIENTED_EDGE('',*,*,#8796,.F.);
#11856=ORIENTED_EDGE('',*,*,#8780,.T.);
#11857=ORIENTED_EDGE('',*,*,#8808,.F.);
#11858=ORIENTED_EDGE('',*,*,#8819,.F.);
#11859=ORIENTED_EDGE('',*,*,#8793,.F.);
#11860=ORIENTED_EDGE('',*,*,#8806,.F.);
#11861=ORIENTED_EDGE('',*,*,#8794,.F.);
#11862=ORIENTED_EDGE('',*,*,#8819,.T.);
#11863=ORIENTED_EDGE('',*,*,#8812,.F.);
#11864=ORIENTED_EDGE('',*,*,#8798,.F.);
#11865=ORIENTED_EDGE('',*,*,#8820,.F.);
#11866=ORIENTED_EDGE('',*,*,#8820,.T.);
#11867=ORIENTED_EDGE('',*,*,#8797,.F.);
#11868=ORIENTED_EDGE('',*,*,#8774,.F.);
#11869=ORIENTED_EDGE('',*,*,#8814,.F.);
#11870=ORIENTED_EDGE('',*,*,#8776,.T.);
#11871=ORIENTED_EDGE('',*,*,#8800,.F.);
#11872=ORIENTED_EDGE('',*,*,#8821,.F.);
#11873=ORIENTED_EDGE('',*,*,#8809,.F.);
#11874=ORIENTED_EDGE('',*,*,#8799,.F.);
#11875=ORIENTED_EDGE('',*,*,#8811,.F.);
#11876=ORIENTED_EDGE('',*,*,#8821,.T.);
#11877=ORIENTED_EDGE('',*,*,#8822,.T.);
#11878=ORIENTED_EDGE('',*,*,#8823,.T.);
#11879=ORIENTED_EDGE('',*,*,#8824,.T.);
#11880=ORIENTED_EDGE('',*,*,#8825,.F.);
#11881=ORIENTED_EDGE('',*,*,#8826,.T.);
#11882=ORIENTED_EDGE('',*,*,#8827,.T.);
#11883=ORIENTED_EDGE('',*,*,#8822,.F.);
#11884=ORIENTED_EDGE('',*,*,#8828,.F.);
#11885=ORIENTED_EDGE('',*,*,#8829,.T.);
#11886=ORIENTED_EDGE('',*,*,#8830,.T.);
#11887=ORIENTED_EDGE('',*,*,#8826,.F.);
#11888=ORIENTED_EDGE('',*,*,#8831,.F.);
#11889=ORIENTED_EDGE('',*,*,#8832,.T.);
#11890=ORIENTED_EDGE('',*,*,#8833,.T.);
#11891=ORIENTED_EDGE('',*,*,#8829,.F.);
#11892=ORIENTED_EDGE('',*,*,#8834,.F.);
#11893=ORIENTED_EDGE('',*,*,#8835,.F.);
#11894=ORIENTED_EDGE('',*,*,#8836,.F.);
#11895=ORIENTED_EDGE('',*,*,#8837,.T.);
#11896=ORIENTED_EDGE('',*,*,#8838,.T.);
#11897=ORIENTED_EDGE('',*,*,#8839,.T.);
#11898=ORIENTED_EDGE('',*,*,#8840,.F.);
#11899=ORIENTED_EDGE('',*,*,#8841,.F.);
#11900=ORIENTED_EDGE('',*,*,#8842,.T.);
#11901=ORIENTED_EDGE('',*,*,#8843,.T.);
#11902=ORIENTED_EDGE('',*,*,#8844,.F.);
#11903=ORIENTED_EDGE('',*,*,#8839,.F.);
#11904=ORIENTED_EDGE('',*,*,#8845,.F.);
#11905=ORIENTED_EDGE('',*,*,#8846,.T.);
#11906=ORIENTED_EDGE('',*,*,#8847,.T.);
#11907=ORIENTED_EDGE('',*,*,#8842,.F.);
#11908=ORIENTED_EDGE('',*,*,#8848,.F.);
#11909=ORIENTED_EDGE('',*,*,#8849,.T.);
#11910=ORIENTED_EDGE('',*,*,#8850,.T.);
#11911=ORIENTED_EDGE('',*,*,#8846,.F.);
#11912=ORIENTED_EDGE('',*,*,#8851,.F.);
#11913=ORIENTED_EDGE('',*,*,#8852,.T.);
#11914=ORIENTED_EDGE('',*,*,#8853,.T.);
#11915=ORIENTED_EDGE('',*,*,#8849,.F.);
#11916=ORIENTED_EDGE('',*,*,#8854,.F.);
#11917=ORIENTED_EDGE('',*,*,#8855,.F.);
#11918=ORIENTED_EDGE('',*,*,#8856,.F.);
#11919=ORIENTED_EDGE('',*,*,#8857,.T.);
#11920=ORIENTED_EDGE('',*,*,#8858,.T.);
#11921=ORIENTED_EDGE('',*,*,#8859,.F.);
#11922=ORIENTED_EDGE('',*,*,#8860,.T.);
#11923=ORIENTED_EDGE('',*,*,#8861,.F.);
#11924=ORIENTED_EDGE('',*,*,#8860,.F.);
#11925=ORIENTED_EDGE('',*,*,#8862,.T.);
#11926=ORIENTED_EDGE('',*,*,#8863,.T.);
#11927=ORIENTED_EDGE('',*,*,#8859,.T.);
#11928=ORIENTED_EDGE('',*,*,#8863,.F.);
#11929=ORIENTED_EDGE('',*,*,#8864,.T.);
#11930=ORIENTED_EDGE('',*,*,#8862,.F.);
#11931=ORIENTED_EDGE('',*,*,#8865,.T.);
#11932=ORIENTED_EDGE('',*,*,#8866,.F.);
#11933=ORIENTED_EDGE('',*,*,#8867,.F.);
#11934=ORIENTED_EDGE('',*,*,#8868,.F.);
#11935=ORIENTED_EDGE('',*,*,#8869,.T.);
#11936=ORIENTED_EDGE('',*,*,#8870,.F.);
#11937=ORIENTED_EDGE('',*,*,#8871,.F.);
#11938=ORIENTED_EDGE('',*,*,#8872,.F.);
#11939=ORIENTED_EDGE('',*,*,#8865,.F.);
#11940=ORIENTED_EDGE('',*,*,#8864,.F.);
#11941=ORIENTED_EDGE('',*,*,#8855,.T.);
#11942=ORIENTED_EDGE('',*,*,#8873,.T.);
#11943=ORIENTED_EDGE('',*,*,#8852,.F.);
#11944=ORIENTED_EDGE('',*,*,#8874,.F.);
#11945=ORIENTED_EDGE('',*,*,#8875,.F.);
#11946=ORIENTED_EDGE('',*,*,#8870,.T.);
#11947=ORIENTED_EDGE('',*,*,#8876,.T.);
#11948=ORIENTED_EDGE('',*,*,#8877,.T.);
#11949=ORIENTED_EDGE('',*,*,#8871,.T.);
#11950=ORIENTED_EDGE('',*,*,#8875,.T.);
#11951=ORIENTED_EDGE('',*,*,#8878,.F.);
#11952=ORIENTED_EDGE('',*,*,#8879,.T.);
#11953=ORIENTED_EDGE('',*,*,#8880,.T.);
#11954=ORIENTED_EDGE('',*,*,#8881,.T.);
#11955=ORIENTED_EDGE('',*,*,#8882,.T.);
#11956=ORIENTED_EDGE('',*,*,#8883,.T.);
#11957=ORIENTED_EDGE('',*,*,#8884,.F.);
#11958=ORIENTED_EDGE('',*,*,#8885,.T.);
#11959=ORIENTED_EDGE('',*,*,#8867,.T.);
#11960=ORIENTED_EDGE('',*,*,#8886,.T.);
#11961=ORIENTED_EDGE('',*,*,#8884,.T.);
#11962=ORIENTED_EDGE('',*,*,#8887,.T.);
#11963=ORIENTED_EDGE('',*,*,#8888,.T.);
#11964=ORIENTED_EDGE('',*,*,#8889,.T.);
#11965=ORIENTED_EDGE('',*,*,#8890,.F.);
#11966=ORIENTED_EDGE('',*,*,#8891,.T.);
#11967=ORIENTED_EDGE('',*,*,#8892,.F.);
#11968=ORIENTED_EDGE('',*,*,#8869,.F.);
#11969=ORIENTED_EDGE('',*,*,#8893,.F.);
#11970=ORIENTED_EDGE('',*,*,#8892,.T.);
#11971=ORIENTED_EDGE('',*,*,#8894,.F.);
#11972=ORIENTED_EDGE('',*,*,#8895,.T.);
#11973=ORIENTED_EDGE('',*,*,#8896,.F.);
#11974=ORIENTED_EDGE('',*,*,#8897,.T.);
#11975=ORIENTED_EDGE('',*,*,#8898,.F.);
#11976=ORIENTED_EDGE('',*,*,#8899,.T.);
#11977=ORIENTED_EDGE('',*,*,#8900,.F.);
#11978=ORIENTED_EDGE('',*,*,#8901,.T.);
#11979=ORIENTED_EDGE('',*,*,#8902,.F.);
#11980=ORIENTED_EDGE('',*,*,#8878,.T.);
#11981=ORIENTED_EDGE('',*,*,#8876,.F.);
#11982=ORIENTED_EDGE('',*,*,#8857,.F.);
#11983=ORIENTED_EDGE('',*,*,#8903,.F.);
#11984=ORIENTED_EDGE('',*,*,#8837,.F.);
#11985=ORIENTED_EDGE('',*,*,#8904,.F.);
#11986=ORIENTED_EDGE('',*,*,#8905,.T.);
#11987=ORIENTED_EDGE('',*,*,#8906,.F.);
#11988=ORIENTED_EDGE('',*,*,#8907,.T.);
#11989=ORIENTED_EDGE('',*,*,#8908,.F.);
#11990=ORIENTED_EDGE('',*,*,#8909,.T.);
#11991=ORIENTED_EDGE('',*,*,#8910,.F.);
#11992=ORIENTED_EDGE('',*,*,#8911,.T.);
#11993=ORIENTED_EDGE('',*,*,#8912,.F.);
#11994=ORIENTED_EDGE('',*,*,#8913,.T.);
#11995=ORIENTED_EDGE('',*,*,#8888,.F.);
#11996=ORIENTED_EDGE('',*,*,#8914,.T.);
#11997=ORIENTED_EDGE('',*,*,#8882,.F.);
#11998=ORIENTED_EDGE('',*,*,#8840,.T.);
#11999=ORIENTED_EDGE('',*,*,#8844,.T.);
#12000=ORIENTED_EDGE('',*,*,#8915,.F.);
#12001=ORIENTED_EDGE('',*,*,#8824,.F.);
#12002=ORIENTED_EDGE('',*,*,#8916,.F.);
#12003=ORIENTED_EDGE('',*,*,#8917,.F.);
#12004=ORIENTED_EDGE('',*,*,#8918,.T.);
#12005=ORIENTED_EDGE('',*,*,#8895,.F.);
#12006=ORIENTED_EDGE('',*,*,#8919,.T.);
#12007=ORIENTED_EDGE('',*,*,#8890,.T.);
#12008=ORIENTED_EDGE('',*,*,#8920,.T.);
#12009=ORIENTED_EDGE('',*,*,#8912,.T.);
#12010=ORIENTED_EDGE('',*,*,#8921,.T.);
#12011=ORIENTED_EDGE('',*,*,#8922,.F.);
#12012=ORIENTED_EDGE('',*,*,#8923,.T.);
#12013=ORIENTED_EDGE('',*,*,#8897,.F.);
#12014=ORIENTED_EDGE('',*,*,#8924,.T.);
#12015=ORIENTED_EDGE('',*,*,#8917,.T.);
#12016=ORIENTED_EDGE('',*,*,#8925,.T.);
#12017=ORIENTED_EDGE('',*,*,#8910,.T.);
#12018=ORIENTED_EDGE('',*,*,#8926,.T.);
#12019=ORIENTED_EDGE('',*,*,#8927,.F.);
#12020=ORIENTED_EDGE('',*,*,#8928,.T.);
#12021=ORIENTED_EDGE('',*,*,#8899,.F.);
#12022=ORIENTED_EDGE('',*,*,#8929,.T.);
#12023=ORIENTED_EDGE('',*,*,#8922,.T.);
#12024=ORIENTED_EDGE('',*,*,#8930,.T.);
#12025=ORIENTED_EDGE('',*,*,#8908,.T.);
#12026=ORIENTED_EDGE('',*,*,#8931,.T.);
#12027=ORIENTED_EDGE('',*,*,#8880,.F.);
#12028=ORIENTED_EDGE('',*,*,#8932,.T.);
#12029=ORIENTED_EDGE('',*,*,#8901,.F.);
#12030=ORIENTED_EDGE('',*,*,#8933,.T.);
#12031=ORIENTED_EDGE('',*,*,#8927,.T.);
#12032=ORIENTED_EDGE('',*,*,#8934,.T.);
#12033=ORIENTED_EDGE('',*,*,#8906,.T.);
#12034=ORIENTED_EDGE('',*,*,#8935,.T.);
#12035=ORIENTED_EDGE('',*,*,#8935,.F.);
#12036=ORIENTED_EDGE('',*,*,#8905,.F.);
#12037=ORIENTED_EDGE('',*,*,#8881,.F.);
#12038=ORIENTED_EDGE('',*,*,#8907,.F.);
#12039=ORIENTED_EDGE('',*,*,#8934,.F.);
#12040=ORIENTED_EDGE('',*,*,#8931,.F.);
#12041=ORIENTED_EDGE('',*,*,#8933,.F.);
#12042=ORIENTED_EDGE('',*,*,#8900,.T.);
#12043=ORIENTED_EDGE('',*,*,#8928,.F.);
#12044=ORIENTED_EDGE('',*,*,#8902,.T.);
#12045=ORIENTED_EDGE('',*,*,#8932,.F.);
#12046=ORIENTED_EDGE('',*,*,#8879,.F.);
#12047=ORIENTED_EDGE('',*,*,#8909,.F.);
#12048=ORIENTED_EDGE('',*,*,#8930,.F.);
#12049=ORIENTED_EDGE('',*,*,#8926,.F.);
#12050=ORIENTED_EDGE('',*,*,#8929,.F.);
#12051=ORIENTED_EDGE('',*,*,#8898,.T.);
#12052=ORIENTED_EDGE('',*,*,#8923,.F.);
#12053=ORIENTED_EDGE('',*,*,#8911,.F.);
#12054=ORIENTED_EDGE('',*,*,#8925,.F.);
#12055=ORIENTED_EDGE('',*,*,#8921,.F.);
#12056=ORIENTED_EDGE('',*,*,#8924,.F.);
#12057=ORIENTED_EDGE('',*,*,#8896,.T.);
#12058=ORIENTED_EDGE('',*,*,#8918,.F.);
#12059=ORIENTED_EDGE('',*,*,#8913,.F.);
#12060=ORIENTED_EDGE('',*,*,#8920,.F.);
#12061=ORIENTED_EDGE('',*,*,#8889,.F.);
#12062=ORIENTED_EDGE('',*,*,#8919,.F.);
#12063=ORIENTED_EDGE('',*,*,#8894,.T.);
#12064=ORIENTED_EDGE('',*,*,#8891,.F.);
#12065=ORIENTED_EDGE('',*,*,#8914,.F.);
#12066=ORIENTED_EDGE('',*,*,#8887,.F.);
#12067=ORIENTED_EDGE('',*,*,#8883,.F.);
#12068=ORIENTED_EDGE('',*,*,#8893,.T.);
#12069=ORIENTED_EDGE('',*,*,#8868,.T.);
#12070=ORIENTED_EDGE('',*,*,#8885,.F.);
#12071=ORIENTED_EDGE('',*,*,#8858,.F.);
#12072=ORIENTED_EDGE('',*,*,#8904,.T.);
#12073=ORIENTED_EDGE('',*,*,#8836,.T.);
#12074=ORIENTED_EDGE('',*,*,#8936,.T.);
#12075=ORIENTED_EDGE('',*,*,#8834,.T.);
#12076=ORIENTED_EDGE('',*,*,#8831,.T.);
#12077=ORIENTED_EDGE('',*,*,#8828,.T.);
#12078=ORIENTED_EDGE('',*,*,#8825,.T.);
#12079=ORIENTED_EDGE('',*,*,#8915,.T.);
#12080=ORIENTED_EDGE('',*,*,#8843,.F.);
#12081=ORIENTED_EDGE('',*,*,#8847,.F.);
#12082=ORIENTED_EDGE('',*,*,#8850,.F.);
#12083=ORIENTED_EDGE('',*,*,#8853,.F.);
#12084=ORIENTED_EDGE('',*,*,#8873,.F.);
#12085=ORIENTED_EDGE('',*,*,#8835,.T.);
#12086=ORIENTED_EDGE('',*,*,#8937,.T.);
#12087=ORIENTED_EDGE('',*,*,#8832,.F.);
#12088=ORIENTED_EDGE('',*,*,#8936,.F.);
#12089=ORIENTED_EDGE('',*,*,#8838,.F.);
#12090=ORIENTED_EDGE('',*,*,#8903,.T.);
#12091=ORIENTED_EDGE('',*,*,#8856,.T.);
#12092=ORIENTED_EDGE('',*,*,#8874,.T.);
#12093=ORIENTED_EDGE('',*,*,#8854,.T.);
#12094=ORIENTED_EDGE('',*,*,#8851,.T.);
#12095=ORIENTED_EDGE('',*,*,#8848,.T.);
#12096=ORIENTED_EDGE('',*,*,#8845,.T.);
#12097=ORIENTED_EDGE('',*,*,#8841,.T.);
#12098=ORIENTED_EDGE('',*,*,#8916,.T.);
#12099=ORIENTED_EDGE('',*,*,#8823,.F.);
#12100=ORIENTED_EDGE('',*,*,#8827,.F.);
#12101=ORIENTED_EDGE('',*,*,#8830,.F.);
#12102=ORIENTED_EDGE('',*,*,#8833,.F.);
#12103=ORIENTED_EDGE('',*,*,#8937,.F.);
#12104=ORIENTED_EDGE('',*,*,#8877,.F.);
#12105=ORIENTED_EDGE('',*,*,#8886,.F.);
#12106=ORIENTED_EDGE('',*,*,#8866,.T.);
#12107=ORIENTED_EDGE('',*,*,#8872,.T.);
#12108=ORIENTED_EDGE('',*,*,#8861,.T.);
#12109=ORIENTED_EDGE('',*,*,#8938,.F.);
#12110=ORIENTED_EDGE('',*,*,#8939,.T.);
#12111=ORIENTED_EDGE('',*,*,#8940,.T.);
#12112=ORIENTED_EDGE('',*,*,#8939,.F.);
#12113=ORIENTED_EDGE('',*,*,#8941,.F.);
#12114=ORIENTED_EDGE('',*,*,#8942,.T.);
#12115=ORIENTED_EDGE('',*,*,#8943,.T.);
#12116=ORIENTED_EDGE('',*,*,#8942,.F.);
#12117=ORIENTED_EDGE('',*,*,#8940,.F.);
#12118=ORIENTED_EDGE('',*,*,#8941,.T.);
#12119=ORIENTED_EDGE('',*,*,#8938,.T.);
#12120=ORIENTED_EDGE('',*,*,#8943,.F.);
#12121=ORIENTED_EDGE('',*,*,#8944,.T.);
#12122=ORIENTED_EDGE('',*,*,#8945,.F.);
#12123=ORIENTED_EDGE('',*,*,#8946,.F.);
#12124=ORIENTED_EDGE('',*,*,#8947,.T.);
#12125=ORIENTED_EDGE('',*,*,#8948,.T.);
#12126=ORIENTED_EDGE('',*,*,#8949,.F.);
#12127=ORIENTED_EDGE('',*,*,#8950,.F.);
#12128=ORIENTED_EDGE('',*,*,#8945,.T.);
#12129=ORIENTED_EDGE('',*,*,#8951,.T.);
#12130=ORIENTED_EDGE('',*,*,#8952,.F.);
#12131=ORIENTED_EDGE('',*,*,#8953,.F.);
#12132=ORIENTED_EDGE('',*,*,#8949,.T.);
#12133=ORIENTED_EDGE('',*,*,#8954,.T.);
#12134=ORIENTED_EDGE('',*,*,#8947,.F.);
#12135=ORIENTED_EDGE('',*,*,#8955,.F.);
#12136=ORIENTED_EDGE('',*,*,#8952,.T.);
#12137=ORIENTED_EDGE('',*,*,#8946,.T.);
#12138=ORIENTED_EDGE('',*,*,#8950,.T.);
#12139=ORIENTED_EDGE('',*,*,#8953,.T.);
#12140=ORIENTED_EDGE('',*,*,#8955,.T.);
#12141=ORIENTED_EDGE('',*,*,#8944,.F.);
#12142=ORIENTED_EDGE('',*,*,#8954,.F.);
#12143=ORIENTED_EDGE('',*,*,#8951,.F.);
#12144=ORIENTED_EDGE('',*,*,#8948,.F.);
#12145=ORIENTED_EDGE('',*,*,#8956,.T.);
#12146=ORIENTED_EDGE('',*,*,#8957,.T.);
#12147=ORIENTED_EDGE('',*,*,#8958,.F.);
#12148=ORIENTED_EDGE('',*,*,#8957,.F.);
#12149=ORIENTED_EDGE('',*,*,#8959,.T.);
#12150=ORIENTED_EDGE('',*,*,#8960,.T.);
#12151=ORIENTED_EDGE('',*,*,#8961,.T.);
#12152=ORIENTED_EDGE('',*,*,#8962,.T.);
#12153=ORIENTED_EDGE('',*,*,#8963,.T.);
#12154=ORIENTED_EDGE('',*,*,#8964,.T.);
#12155=ORIENTED_EDGE('',*,*,#8956,.F.);
#12156=ORIENTED_EDGE('',*,*,#8965,.F.);
#12157=ORIENTED_EDGE('',*,*,#8966,.F.);
#12158=ORIENTED_EDGE('',*,*,#8967,.F.);
#12159=ORIENTED_EDGE('',*,*,#8968,.F.);
#12160=ORIENTED_EDGE('',*,*,#8969,.F.);
#12161=ORIENTED_EDGE('',*,*,#8970,.F.);
#12162=ORIENTED_EDGE('',*,*,#8958,.T.);
#12163=ORIENTED_EDGE('',*,*,#8965,.T.);
#12164=ORIENTED_EDGE('',*,*,#8971,.F.);
#12165=ORIENTED_EDGE('',*,*,#8959,.F.);
#12166=ORIENTED_EDGE('',*,*,#8972,.T.);
#12167=ORIENTED_EDGE('',*,*,#8970,.T.);
#12168=ORIENTED_EDGE('',*,*,#8973,.F.);
#12169=ORIENTED_EDGE('',*,*,#8960,.F.);
#12170=ORIENTED_EDGE('',*,*,#8971,.T.);
#12171=ORIENTED_EDGE('',*,*,#8969,.T.);
#12172=ORIENTED_EDGE('',*,*,#8974,.F.);
#12173=ORIENTED_EDGE('',*,*,#8961,.F.);
#12174=ORIENTED_EDGE('',*,*,#8973,.T.);
#12175=ORIENTED_EDGE('',*,*,#8968,.T.);
#12176=ORIENTED_EDGE('',*,*,#8975,.F.);
#12177=ORIENTED_EDGE('',*,*,#8962,.F.);
#12178=ORIENTED_EDGE('',*,*,#8974,.T.);
#12179=ORIENTED_EDGE('',*,*,#8967,.T.);
#12180=ORIENTED_EDGE('',*,*,#8976,.F.);
#12181=ORIENTED_EDGE('',*,*,#8963,.F.);
#12182=ORIENTED_EDGE('',*,*,#8975,.T.);
#12183=ORIENTED_EDGE('',*,*,#8966,.T.);
#12184=ORIENTED_EDGE('',*,*,#8972,.F.);
#12185=ORIENTED_EDGE('',*,*,#8964,.F.);
#12186=ORIENTED_EDGE('',*,*,#8976,.T.);
#12187=ORIENTED_EDGE('',*,*,#8977,.F.);
#12188=ORIENTED_EDGE('',*,*,#8978,.T.);
#12189=ORIENTED_EDGE('',*,*,#8979,.T.);
#12190=ORIENTED_EDGE('',*,*,#8978,.F.);
#12191=ORIENTED_EDGE('',*,*,#8980,.F.);
#12192=ORIENTED_EDGE('',*,*,#8981,.F.);
#12193=ORIENTED_EDGE('',*,*,#8982,.F.);
#12194=ORIENTED_EDGE('',*,*,#8983,.F.);
#12195=ORIENTED_EDGE('',*,*,#8984,.F.);
#12196=ORIENTED_EDGE('',*,*,#8985,.F.);
#12197=ORIENTED_EDGE('',*,*,#8977,.T.);
#12198=ORIENTED_EDGE('',*,*,#8986,.T.);
#12199=ORIENTED_EDGE('',*,*,#8987,.T.);
#12200=ORIENTED_EDGE('',*,*,#8988,.T.);
#12201=ORIENTED_EDGE('',*,*,#8989,.T.);
#12202=ORIENTED_EDGE('',*,*,#8990,.T.);
#12203=ORIENTED_EDGE('',*,*,#8991,.T.);
#12204=ORIENTED_EDGE('',*,*,#8979,.F.);
#12205=ORIENTED_EDGE('',*,*,#8986,.F.);
#12206=ORIENTED_EDGE('',*,*,#8992,.F.);
#12207=ORIENTED_EDGE('',*,*,#8980,.T.);
#12208=ORIENTED_EDGE('',*,*,#8993,.T.);
#12209=ORIENTED_EDGE('',*,*,#8987,.F.);
#12210=ORIENTED_EDGE('',*,*,#8993,.F.);
#12211=ORIENTED_EDGE('',*,*,#8985,.T.);
#12212=ORIENTED_EDGE('',*,*,#8994,.T.);
#12213=ORIENTED_EDGE('',*,*,#8988,.F.);
#12214=ORIENTED_EDGE('',*,*,#8994,.F.);
#12215=ORIENTED_EDGE('',*,*,#8984,.T.);
#12216=ORIENTED_EDGE('',*,*,#8995,.T.);
#12217=ORIENTED_EDGE('',*,*,#8989,.F.);
#12218=ORIENTED_EDGE('',*,*,#8995,.F.);
#12219=ORIENTED_EDGE('',*,*,#8983,.T.);
#12220=ORIENTED_EDGE('',*,*,#8996,.T.);
#12221=ORIENTED_EDGE('',*,*,#8990,.F.);
#12222=ORIENTED_EDGE('',*,*,#8996,.F.);
#12223=ORIENTED_EDGE('',*,*,#8982,.T.);
#12224=ORIENTED_EDGE('',*,*,#8997,.T.);
#12225=ORIENTED_EDGE('',*,*,#8991,.F.);
#12226=ORIENTED_EDGE('',*,*,#8997,.F.);
#12227=ORIENTED_EDGE('',*,*,#8981,.T.);
#12228=ORIENTED_EDGE('',*,*,#8992,.T.);
#12229=ORIENTED_EDGE('',*,*,#8998,.T.);
#12230=ORIENTED_EDGE('',*,*,#8999,.T.);
#12231=ORIENTED_EDGE('',*,*,#9000,.F.);
#12232=ORIENTED_EDGE('',*,*,#8999,.F.);
#12233=ORIENTED_EDGE('',*,*,#9001,.T.);
#12234=ORIENTED_EDGE('',*,*,#9002,.T.);
#12235=ORIENTED_EDGE('',*,*,#9003,.F.);
#12236=ORIENTED_EDGE('',*,*,#9002,.F.);
#12237=ORIENTED_EDGE('',*,*,#9004,.T.);
#12238=ORIENTED_EDGE('',*,*,#9005,.T.);
#12239=ORIENTED_EDGE('',*,*,#9006,.F.);
#12240=ORIENTED_EDGE('',*,*,#9005,.F.);
#12241=ORIENTED_EDGE('',*,*,#9007,.T.);
#12242=ORIENTED_EDGE('',*,*,#9008,.T.);
#12243=ORIENTED_EDGE('',*,*,#9009,.F.);
#12244=ORIENTED_EDGE('',*,*,#9008,.F.);
#12245=ORIENTED_EDGE('',*,*,#9010,.T.);
#12246=ORIENTED_EDGE('',*,*,#9011,.T.);
#12247=ORIENTED_EDGE('',*,*,#9012,.F.);
#12248=ORIENTED_EDGE('',*,*,#9011,.F.);
#12249=ORIENTED_EDGE('',*,*,#9013,.T.);
#12250=ORIENTED_EDGE('',*,*,#9014,.T.);
#12251=ORIENTED_EDGE('',*,*,#9015,.T.);
#12252=ORIENTED_EDGE('',*,*,#9016,.T.);
#12253=ORIENTED_EDGE('',*,*,#9017,.T.);
#12254=ORIENTED_EDGE('',*,*,#9018,.T.);
#12255=ORIENTED_EDGE('',*,*,#9019,.T.);
#12256=ORIENTED_EDGE('',*,*,#9020,.T.);
#12257=ORIENTED_EDGE('',*,*,#9010,.F.);
#12258=ORIENTED_EDGE('',*,*,#9007,.F.);
#12259=ORIENTED_EDGE('',*,*,#9004,.F.);
#12260=ORIENTED_EDGE('',*,*,#9001,.F.);
#12261=ORIENTED_EDGE('',*,*,#8998,.F.);
#12262=ORIENTED_EDGE('',*,*,#9021,.F.);
#12263=ORIENTED_EDGE('',*,*,#9022,.F.);
#12264=ORIENTED_EDGE('',*,*,#9023,.F.);
#12265=ORIENTED_EDGE('',*,*,#9024,.F.);
#12266=ORIENTED_EDGE('',*,*,#9025,.F.);
#12267=ORIENTED_EDGE('',*,*,#9026,.F.);
#12268=ORIENTED_EDGE('',*,*,#9027,.F.);
#12269=ORIENTED_EDGE('',*,*,#9028,.F.);
#12270=ORIENTED_EDGE('',*,*,#9012,.T.);
#12271=ORIENTED_EDGE('',*,*,#9006,.T.);
#12272=ORIENTED_EDGE('',*,*,#9000,.T.);
#12273=ORIENTED_EDGE('',*,*,#9003,.T.);
#12274=ORIENTED_EDGE('',*,*,#9009,.T.);
#12275=ORIENTED_EDGE('',*,*,#9021,.T.);
#12276=ORIENTED_EDGE('',*,*,#9029,.F.);
#12277=ORIENTED_EDGE('',*,*,#9013,.F.);
#12278=ORIENTED_EDGE('',*,*,#9030,.T.);
#12279=ORIENTED_EDGE('',*,*,#9028,.T.);
#12280=ORIENTED_EDGE('',*,*,#9031,.F.);
#12281=ORIENTED_EDGE('',*,*,#9014,.F.);
#12282=ORIENTED_EDGE('',*,*,#9029,.T.);
#12283=ORIENTED_EDGE('',*,*,#9027,.T.);
#12284=ORIENTED_EDGE('',*,*,#9032,.F.);
#12285=ORIENTED_EDGE('',*,*,#9015,.F.);
#12286=ORIENTED_EDGE('',*,*,#9031,.T.);
#12287=ORIENTED_EDGE('',*,*,#9026,.T.);
#12288=ORIENTED_EDGE('',*,*,#9033,.F.);
#12289=ORIENTED_EDGE('',*,*,#9016,.F.);
#12290=ORIENTED_EDGE('',*,*,#9032,.T.);
#12291=ORIENTED_EDGE('',*,*,#9025,.T.);
#12292=ORIENTED_EDGE('',*,*,#9034,.F.);
#12293=ORIENTED_EDGE('',*,*,#9017,.F.);
#12294=ORIENTED_EDGE('',*,*,#9033,.T.);
#12295=ORIENTED_EDGE('',*,*,#9024,.T.);
#12296=ORIENTED_EDGE('',*,*,#9035,.F.);
#12297=ORIENTED_EDGE('',*,*,#9018,.F.);
#12298=ORIENTED_EDGE('',*,*,#9034,.T.);
#12299=ORIENTED_EDGE('',*,*,#9023,.T.);
#12300=ORIENTED_EDGE('',*,*,#9036,.F.);
#12301=ORIENTED_EDGE('',*,*,#9019,.F.);
#12302=ORIENTED_EDGE('',*,*,#9035,.T.);
#12303=ORIENTED_EDGE('',*,*,#9022,.T.);
#12304=ORIENTED_EDGE('',*,*,#9030,.F.);
#12305=ORIENTED_EDGE('',*,*,#9020,.F.);
#12306=ORIENTED_EDGE('',*,*,#9036,.T.);
#12307=ORIENTED_EDGE('',*,*,#9037,.T.);
#12308=ORIENTED_EDGE('',*,*,#9038,.F.);
#12309=ORIENTED_EDGE('',*,*,#9039,.F.);
#12310=ORIENTED_EDGE('',*,*,#9040,.T.);
#12311=ORIENTED_EDGE('',*,*,#9041,.T.);
#12312=ORIENTED_EDGE('',*,*,#9042,.F.);
#12313=ORIENTED_EDGE('',*,*,#9043,.F.);
#12314=ORIENTED_EDGE('',*,*,#9038,.T.);
#12315=ORIENTED_EDGE('',*,*,#9044,.T.);
#12316=ORIENTED_EDGE('',*,*,#9045,.F.);
#12317=ORIENTED_EDGE('',*,*,#9046,.F.);
#12318=ORIENTED_EDGE('',*,*,#9042,.T.);
#12319=ORIENTED_EDGE('',*,*,#9047,.T.);
#12320=ORIENTED_EDGE('',*,*,#9040,.F.);
#12321=ORIENTED_EDGE('',*,*,#9048,.F.);
#12322=ORIENTED_EDGE('',*,*,#9045,.T.);
#12323=ORIENTED_EDGE('',*,*,#9039,.T.);
#12324=ORIENTED_EDGE('',*,*,#9043,.T.);
#12325=ORIENTED_EDGE('',*,*,#9046,.T.);
#12326=ORIENTED_EDGE('',*,*,#9048,.T.);
#12327=ORIENTED_EDGE('',*,*,#9037,.F.);
#12328=ORIENTED_EDGE('',*,*,#9047,.F.);
#12329=ORIENTED_EDGE('',*,*,#9044,.F.);
#12330=ORIENTED_EDGE('',*,*,#9041,.F.);
#12331=ORIENTED_EDGE('',*,*,#9049,.T.);
#12332=ORIENTED_EDGE('',*,*,#9050,.F.);
#12333=ORIENTED_EDGE('',*,*,#9051,.F.);
#12334=ORIENTED_EDGE('',*,*,#9052,.T.);
#12335=ORIENTED_EDGE('',*,*,#9053,.T.);
#12336=ORIENTED_EDGE('',*,*,#9054,.F.);
#12337=ORIENTED_EDGE('',*,*,#9055,.F.);
#12338=ORIENTED_EDGE('',*,*,#9050,.T.);
#12339=ORIENTED_EDGE('',*,*,#9056,.T.);
#12340=ORIENTED_EDGE('',*,*,#9057,.F.);
#12341=ORIENTED_EDGE('',*,*,#9058,.F.);
#12342=ORIENTED_EDGE('',*,*,#9054,.T.);
#12343=ORIENTED_EDGE('',*,*,#9059,.T.);
#12344=ORIENTED_EDGE('',*,*,#9052,.F.);
#12345=ORIENTED_EDGE('',*,*,#9060,.F.);
#12346=ORIENTED_EDGE('',*,*,#9057,.T.);
#12347=ORIENTED_EDGE('',*,*,#9051,.T.);
#12348=ORIENTED_EDGE('',*,*,#9055,.T.);
#12349=ORIENTED_EDGE('',*,*,#9058,.T.);
#12350=ORIENTED_EDGE('',*,*,#9060,.T.);
#12351=ORIENTED_EDGE('',*,*,#9049,.F.);
#12352=ORIENTED_EDGE('',*,*,#9059,.F.);
#12353=ORIENTED_EDGE('',*,*,#9056,.F.);
#12354=ORIENTED_EDGE('',*,*,#9053,.F.);
#12355=ORIENTED_EDGE('',*,*,#9061,.T.);
#12356=ORIENTED_EDGE('',*,*,#9062,.F.);
#12357=ORIENTED_EDGE('',*,*,#9063,.F.);
#12358=ORIENTED_EDGE('',*,*,#9064,.T.);
#12359=ORIENTED_EDGE('',*,*,#9065,.T.);
#12360=ORIENTED_EDGE('',*,*,#9066,.F.);
#12361=ORIENTED_EDGE('',*,*,#9067,.F.);
#12362=ORIENTED_EDGE('',*,*,#9062,.T.);
#12363=ORIENTED_EDGE('',*,*,#9068,.T.);
#12364=ORIENTED_EDGE('',*,*,#9069,.F.);
#12365=ORIENTED_EDGE('',*,*,#9070,.F.);
#12366=ORIENTED_EDGE('',*,*,#9066,.T.);
#12367=ORIENTED_EDGE('',*,*,#9071,.T.);
#12368=ORIENTED_EDGE('',*,*,#9072,.F.);
#12369=ORIENTED_EDGE('',*,*,#9073,.F.);
#12370=ORIENTED_EDGE('',*,*,#9069,.T.);
#12371=ORIENTED_EDGE('',*,*,#9074,.T.);
#12372=ORIENTED_EDGE('',*,*,#9075,.F.);
#12373=ORIENTED_EDGE('',*,*,#9076,.F.);
#12374=ORIENTED_EDGE('',*,*,#9072,.T.);
#12375=ORIENTED_EDGE('',*,*,#9077,.T.);
#12376=ORIENTED_EDGE('',*,*,#9064,.F.);
#12377=ORIENTED_EDGE('',*,*,#9078,.F.);
#12378=ORIENTED_EDGE('',*,*,#9075,.T.);
#12379=ORIENTED_EDGE('',*,*,#9063,.T.);
#12380=ORIENTED_EDGE('',*,*,#9067,.T.);
#12381=ORIENTED_EDGE('',*,*,#9070,.T.);
#12382=ORIENTED_EDGE('',*,*,#9073,.T.);
#12383=ORIENTED_EDGE('',*,*,#9076,.T.);
#12384=ORIENTED_EDGE('',*,*,#9078,.T.);
#12385=ORIENTED_EDGE('',*,*,#9061,.F.);
#12386=ORIENTED_EDGE('',*,*,#9077,.F.);
#12387=ORIENTED_EDGE('',*,*,#9074,.F.);
#12388=ORIENTED_EDGE('',*,*,#9071,.F.);
#12389=ORIENTED_EDGE('',*,*,#9068,.F.);
#12390=ORIENTED_EDGE('',*,*,#9065,.F.);
#12391=ORIENTED_EDGE('',*,*,#9079,.T.);
#12392=ORIENTED_EDGE('',*,*,#9080,.T.);
#12393=ORIENTED_EDGE('',*,*,#9081,.F.);
#12394=ORIENTED_EDGE('',*,*,#9080,.F.);
#12395=ORIENTED_EDGE('',*,*,#9082,.T.);
#12396=ORIENTED_EDGE('',*,*,#9083,.T.);
#12397=ORIENTED_EDGE('',*,*,#9084,.F.);
#12398=ORIENTED_EDGE('',*,*,#9083,.F.);
#12399=ORIENTED_EDGE('',*,*,#9085,.T.);
#12400=ORIENTED_EDGE('',*,*,#9086,.T.);
#12401=ORIENTED_EDGE('',*,*,#9087,.F.);
#12402=ORIENTED_EDGE('',*,*,#9086,.F.);
#12403=ORIENTED_EDGE('',*,*,#9088,.T.);
#12404=ORIENTED_EDGE('',*,*,#9089,.T.);
#12405=ORIENTED_EDGE('',*,*,#9090,.T.);
#12406=ORIENTED_EDGE('',*,*,#9091,.T.);
#12407=ORIENTED_EDGE('',*,*,#9085,.F.);
#12408=ORIENTED_EDGE('',*,*,#9079,.F.);
#12409=ORIENTED_EDGE('',*,*,#9082,.F.);
#12410=ORIENTED_EDGE('',*,*,#9092,.F.);
#12411=ORIENTED_EDGE('',*,*,#9093,.F.);
#12412=ORIENTED_EDGE('',*,*,#9094,.F.);
#12413=ORIENTED_EDGE('',*,*,#9095,.F.);
#12414=ORIENTED_EDGE('',*,*,#9087,.T.);
#12415=ORIENTED_EDGE('',*,*,#9084,.T.);
#12416=ORIENTED_EDGE('',*,*,#9081,.T.);
#12417=ORIENTED_EDGE('',*,*,#9092,.T.);
#12418=ORIENTED_EDGE('',*,*,#9096,.F.);
#12419=ORIENTED_EDGE('',*,*,#9088,.F.);
#12420=ORIENTED_EDGE('',*,*,#9097,.T.);
#12421=ORIENTED_EDGE('',*,*,#9095,.T.);
#12422=ORIENTED_EDGE('',*,*,#9098,.F.);
#12423=ORIENTED_EDGE('',*,*,#9089,.F.);
#12424=ORIENTED_EDGE('',*,*,#9096,.T.);
#12425=ORIENTED_EDGE('',*,*,#9094,.T.);
#12426=ORIENTED_EDGE('',*,*,#9099,.F.);
#12427=ORIENTED_EDGE('',*,*,#9090,.F.);
#12428=ORIENTED_EDGE('',*,*,#9098,.T.);
#12429=ORIENTED_EDGE('',*,*,#9093,.T.);
#12430=ORIENTED_EDGE('',*,*,#9097,.F.);
#12431=ORIENTED_EDGE('',*,*,#9091,.F.);
#12432=ORIENTED_EDGE('',*,*,#9099,.T.);
#12433=ORIENTED_EDGE('',*,*,#9100,.T.);
#12434=ORIENTED_EDGE('',*,*,#9101,.T.);
#12435=ORIENTED_EDGE('',*,*,#9102,.F.);
#12436=ORIENTED_EDGE('',*,*,#9101,.F.);
#12437=ORIENTED_EDGE('',*,*,#9103,.T.);
#12438=ORIENTED_EDGE('',*,*,#9104,.T.);
#12439=ORIENTED_EDGE('',*,*,#9105,.F.);
#12440=ORIENTED_EDGE('',*,*,#9104,.F.);
#12441=ORIENTED_EDGE('',*,*,#9106,.T.);
#12442=ORIENTED_EDGE('',*,*,#9107,.T.);
#12443=ORIENTED_EDGE('',*,*,#9108,.F.);
#12444=ORIENTED_EDGE('',*,*,#9107,.F.);
#12445=ORIENTED_EDGE('',*,*,#9109,.T.);
#12446=ORIENTED_EDGE('',*,*,#9110,.T.);
#12447=ORIENTED_EDGE('',*,*,#9111,.T.);
#12448=ORIENTED_EDGE('',*,*,#9112,.T.);
#12449=ORIENTED_EDGE('',*,*,#9106,.F.);
#12450=ORIENTED_EDGE('',*,*,#9100,.F.);
#12451=ORIENTED_EDGE('',*,*,#9103,.F.);
#12452=ORIENTED_EDGE('',*,*,#9113,.F.);
#12453=ORIENTED_EDGE('',*,*,#9114,.F.);
#12454=ORIENTED_EDGE('',*,*,#9115,.F.);
#12455=ORIENTED_EDGE('',*,*,#9116,.F.);
#12456=ORIENTED_EDGE('',*,*,#9108,.T.);
#12457=ORIENTED_EDGE('',*,*,#9105,.T.);
#12458=ORIENTED_EDGE('',*,*,#9102,.T.);
#12459=ORIENTED_EDGE('',*,*,#9113,.T.);
#12460=ORIENTED_EDGE('',*,*,#9117,.F.);
#12461=ORIENTED_EDGE('',*,*,#9109,.F.);
#12462=ORIENTED_EDGE('',*,*,#9118,.T.);
#12463=ORIENTED_EDGE('',*,*,#9116,.T.);
#12464=ORIENTED_EDGE('',*,*,#9119,.F.);
#12465=ORIENTED_EDGE('',*,*,#9110,.F.);
#12466=ORIENTED_EDGE('',*,*,#9117,.T.);
#12467=ORIENTED_EDGE('',*,*,#9115,.T.);
#12468=ORIENTED_EDGE('',*,*,#9120,.F.);
#12469=ORIENTED_EDGE('',*,*,#9111,.F.);
#12470=ORIENTED_EDGE('',*,*,#9119,.T.);
#12471=ORIENTED_EDGE('',*,*,#9114,.T.);
#12472=ORIENTED_EDGE('',*,*,#9118,.F.);
#12473=ORIENTED_EDGE('',*,*,#9112,.F.);
#12474=ORIENTED_EDGE('',*,*,#9120,.T.);
#12475=ORIENTED_EDGE('',*,*,#9121,.T.);
#12476=ORIENTED_EDGE('',*,*,#9122,.T.);
#12477=ORIENTED_EDGE('',*,*,#9123,.F.);
#12478=ORIENTED_EDGE('',*,*,#9122,.F.);
#12479=ORIENTED_EDGE('',*,*,#9124,.T.);
#12480=ORIENTED_EDGE('',*,*,#9125,.T.);
#12481=ORIENTED_EDGE('',*,*,#9126,.F.);
#12482=ORIENTED_EDGE('',*,*,#9125,.F.);
#12483=ORIENTED_EDGE('',*,*,#9127,.T.);
#12484=ORIENTED_EDGE('',*,*,#9128,.T.);
#12485=ORIENTED_EDGE('',*,*,#9129,.F.);
#12486=ORIENTED_EDGE('',*,*,#9128,.F.);
#12487=ORIENTED_EDGE('',*,*,#9130,.T.);
#12488=ORIENTED_EDGE('',*,*,#9131,.T.);
#12489=ORIENTED_EDGE('',*,*,#9132,.T.);
#12490=ORIENTED_EDGE('',*,*,#9133,.T.);
#12491=ORIENTED_EDGE('',*,*,#9127,.F.);
#12492=ORIENTED_EDGE('',*,*,#9121,.F.);
#12493=ORIENTED_EDGE('',*,*,#9124,.F.);
#12494=ORIENTED_EDGE('',*,*,#9134,.F.);
#12495=ORIENTED_EDGE('',*,*,#9135,.F.);
#12496=ORIENTED_EDGE('',*,*,#9136,.F.);
#12497=ORIENTED_EDGE('',*,*,#9137,.F.);
#12498=ORIENTED_EDGE('',*,*,#9129,.T.);
#12499=ORIENTED_EDGE('',*,*,#9126,.T.);
#12500=ORIENTED_EDGE('',*,*,#9123,.T.);
#12501=ORIENTED_EDGE('',*,*,#9134,.T.);
#12502=ORIENTED_EDGE('',*,*,#9138,.F.);
#12503=ORIENTED_EDGE('',*,*,#9130,.F.);
#12504=ORIENTED_EDGE('',*,*,#9139,.T.);
#12505=ORIENTED_EDGE('',*,*,#9137,.T.);
#12506=ORIENTED_EDGE('',*,*,#9140,.F.);
#12507=ORIENTED_EDGE('',*,*,#9131,.F.);
#12508=ORIENTED_EDGE('',*,*,#9138,.T.);
#12509=ORIENTED_EDGE('',*,*,#9136,.T.);
#12510=ORIENTED_EDGE('',*,*,#9141,.F.);
#12511=ORIENTED_EDGE('',*,*,#9132,.F.);
#12512=ORIENTED_EDGE('',*,*,#9140,.T.);
#12513=ORIENTED_EDGE('',*,*,#9135,.T.);
#12514=ORIENTED_EDGE('',*,*,#9139,.F.);
#12515=ORIENTED_EDGE('',*,*,#9133,.F.);
#12516=ORIENTED_EDGE('',*,*,#9141,.T.);
#12517=ORIENTED_EDGE('',*,*,#9142,.T.);
#12518=ORIENTED_EDGE('',*,*,#9143,.T.);
#12519=ORIENTED_EDGE('',*,*,#9144,.F.);
#12520=ORIENTED_EDGE('',*,*,#9143,.F.);
#12521=ORIENTED_EDGE('',*,*,#9145,.T.);
#12522=ORIENTED_EDGE('',*,*,#9146,.T.);
#12523=ORIENTED_EDGE('',*,*,#9147,.F.);
#12524=ORIENTED_EDGE('',*,*,#9146,.F.);
#12525=ORIENTED_EDGE('',*,*,#9148,.T.);
#12526=ORIENTED_EDGE('',*,*,#9149,.T.);
#12527=ORIENTED_EDGE('',*,*,#9150,.F.);
#12528=ORIENTED_EDGE('',*,*,#9149,.F.);
#12529=ORIENTED_EDGE('',*,*,#9151,.T.);
#12530=ORIENTED_EDGE('',*,*,#9152,.T.);
#12531=ORIENTED_EDGE('',*,*,#9153,.T.);
#12532=ORIENTED_EDGE('',*,*,#9154,.T.);
#12533=ORIENTED_EDGE('',*,*,#9148,.F.);
#12534=ORIENTED_EDGE('',*,*,#9142,.F.);
#12535=ORIENTED_EDGE('',*,*,#9145,.F.);
#12536=ORIENTED_EDGE('',*,*,#9155,.F.);
#12537=ORIENTED_EDGE('',*,*,#9156,.F.);
#12538=ORIENTED_EDGE('',*,*,#9157,.F.);
#12539=ORIENTED_EDGE('',*,*,#9158,.F.);
#12540=ORIENTED_EDGE('',*,*,#9150,.T.);
#12541=ORIENTED_EDGE('',*,*,#9147,.T.);
#12542=ORIENTED_EDGE('',*,*,#9144,.T.);
#12543=ORIENTED_EDGE('',*,*,#9155,.T.);
#12544=ORIENTED_EDGE('',*,*,#9159,.F.);
#12545=ORIENTED_EDGE('',*,*,#9151,.F.);
#12546=ORIENTED_EDGE('',*,*,#9160,.T.);
#12547=ORIENTED_EDGE('',*,*,#9158,.T.);
#12548=ORIENTED_EDGE('',*,*,#9161,.F.);
#12549=ORIENTED_EDGE('',*,*,#9152,.F.);
#12550=ORIENTED_EDGE('',*,*,#9159,.T.);
#12551=ORIENTED_EDGE('',*,*,#9157,.T.);
#12552=ORIENTED_EDGE('',*,*,#9162,.F.);
#12553=ORIENTED_EDGE('',*,*,#9153,.F.);
#12554=ORIENTED_EDGE('',*,*,#9161,.T.);
#12555=ORIENTED_EDGE('',*,*,#9156,.T.);
#12556=ORIENTED_EDGE('',*,*,#9160,.F.);
#12557=ORIENTED_EDGE('',*,*,#9154,.F.);
#12558=ORIENTED_EDGE('',*,*,#9162,.T.);
#12559=ORIENTED_EDGE('',*,*,#9163,.F.);
#12560=ORIENTED_EDGE('',*,*,#9164,.F.);
#12561=ORIENTED_EDGE('',*,*,#9165,.T.);
#12562=ORIENTED_EDGE('',*,*,#9166,.T.);
#12563=ORIENTED_EDGE('',*,*,#9167,.F.);
#12564=ORIENTED_EDGE('',*,*,#9166,.F.);
#12565=ORIENTED_EDGE('',*,*,#9168,.T.);
#12566=ORIENTED_EDGE('',*,*,#9169,.T.);
#12567=ORIENTED_EDGE('',*,*,#9170,.F.);
#12568=ORIENTED_EDGE('',*,*,#9169,.F.);
#12569=ORIENTED_EDGE('',*,*,#9171,.T.);
#12570=ORIENTED_EDGE('',*,*,#9172,.T.);
#12571=ORIENTED_EDGE('',*,*,#9173,.F.);
#12572=ORIENTED_EDGE('',*,*,#9172,.F.);
#12573=ORIENTED_EDGE('',*,*,#9174,.T.);
#12574=ORIENTED_EDGE('',*,*,#9164,.T.);
#12575=ORIENTED_EDGE('',*,*,#9165,.F.);
#12576=ORIENTED_EDGE('',*,*,#9174,.F.);
#12577=ORIENTED_EDGE('',*,*,#9171,.F.);
#12578=ORIENTED_EDGE('',*,*,#9168,.F.);
#12579=ORIENTED_EDGE('',*,*,#9163,.T.);
#12580=ORIENTED_EDGE('',*,*,#9167,.T.);
#12581=ORIENTED_EDGE('',*,*,#9170,.T.);
#12582=ORIENTED_EDGE('',*,*,#9173,.T.);
#12583=ORIENTED_EDGE('',*,*,#9175,.F.);
#12584=ORIENTED_EDGE('',*,*,#9176,.F.);
#12585=ORIENTED_EDGE('',*,*,#9177,.T.);
#12586=ORIENTED_EDGE('',*,*,#9178,.T.);
#12587=ORIENTED_EDGE('',*,*,#9179,.F.);
#12588=ORIENTED_EDGE('',*,*,#9178,.F.);
#12589=ORIENTED_EDGE('',*,*,#9180,.T.);
#12590=ORIENTED_EDGE('',*,*,#9181,.T.);
#12591=ORIENTED_EDGE('',*,*,#9182,.F.);
#12592=ORIENTED_EDGE('',*,*,#9181,.F.);
#12593=ORIENTED_EDGE('',*,*,#9183,.T.);
#12594=ORIENTED_EDGE('',*,*,#9184,.T.);
#12595=ORIENTED_EDGE('',*,*,#9185,.F.);
#12596=ORIENTED_EDGE('',*,*,#9184,.F.);
#12597=ORIENTED_EDGE('',*,*,#9186,.T.);
#12598=ORIENTED_EDGE('',*,*,#9176,.T.);
#12599=ORIENTED_EDGE('',*,*,#9177,.F.);
#12600=ORIENTED_EDGE('',*,*,#9186,.F.);
#12601=ORIENTED_EDGE('',*,*,#9183,.F.);
#12602=ORIENTED_EDGE('',*,*,#9180,.F.);
#12603=ORIENTED_EDGE('',*,*,#9175,.T.);
#12604=ORIENTED_EDGE('',*,*,#9179,.T.);
#12605=ORIENTED_EDGE('',*,*,#9182,.T.);
#12606=ORIENTED_EDGE('',*,*,#9185,.T.);
#12607=ORIENTED_EDGE('',*,*,#9187,.F.);
#12608=ORIENTED_EDGE('',*,*,#9188,.F.);
#12609=ORIENTED_EDGE('',*,*,#9189,.T.);
#12610=ORIENTED_EDGE('',*,*,#9190,.T.);
#12611=ORIENTED_EDGE('',*,*,#9191,.F.);
#12612=ORIENTED_EDGE('',*,*,#9192,.F.);
#12613=ORIENTED_EDGE('',*,*,#9193,.T.);
#12614=ORIENTED_EDGE('',*,*,#9188,.T.);
#12615=ORIENTED_EDGE('',*,*,#9194,.F.);
#12616=ORIENTED_EDGE('',*,*,#9195,.F.);
#12617=ORIENTED_EDGE('',*,*,#9196,.T.);
#12618=ORIENTED_EDGE('',*,*,#9192,.T.);
#12619=ORIENTED_EDGE('',*,*,#9197,.F.);
#12620=ORIENTED_EDGE('',*,*,#9190,.F.);
#12621=ORIENTED_EDGE('',*,*,#9198,.T.);
#12622=ORIENTED_EDGE('',*,*,#9195,.T.);
#12623=ORIENTED_EDGE('',*,*,#9189,.F.);
#12624=ORIENTED_EDGE('',*,*,#9193,.F.);
#12625=ORIENTED_EDGE('',*,*,#9196,.F.);
#12626=ORIENTED_EDGE('',*,*,#9198,.F.);
#12627=ORIENTED_EDGE('',*,*,#9187,.T.);
#12628=ORIENTED_EDGE('',*,*,#9197,.T.);
#12629=ORIENTED_EDGE('',*,*,#9194,.T.);
#12630=ORIENTED_EDGE('',*,*,#9191,.T.);
#12631=ORIENTED_EDGE('',*,*,#9199,.F.);
#12632=ORIENTED_EDGE('',*,*,#9200,.F.);
#12633=ORIENTED_EDGE('',*,*,#9201,.T.);
#12634=ORIENTED_EDGE('',*,*,#9202,.T.);
#12635=ORIENTED_EDGE('',*,*,#9203,.F.);
#12636=ORIENTED_EDGE('',*,*,#9204,.F.);
#12637=ORIENTED_EDGE('',*,*,#9205,.T.);
#12638=ORIENTED_EDGE('',*,*,#9200,.T.);
#12639=ORIENTED_EDGE('',*,*,#9206,.F.);
#12640=ORIENTED_EDGE('',*,*,#9207,.F.);
#12641=ORIENTED_EDGE('',*,*,#9208,.T.);
#12642=ORIENTED_EDGE('',*,*,#9204,.T.);
#12643=ORIENTED_EDGE('',*,*,#9209,.F.);
#12644=ORIENTED_EDGE('',*,*,#9202,.F.);
#12645=ORIENTED_EDGE('',*,*,#9210,.T.);
#12646=ORIENTED_EDGE('',*,*,#9207,.T.);
#12647=ORIENTED_EDGE('',*,*,#9201,.F.);
#12648=ORIENTED_EDGE('',*,*,#9205,.F.);
#12649=ORIENTED_EDGE('',*,*,#9208,.F.);
#12650=ORIENTED_EDGE('',*,*,#9210,.F.);
#12651=ORIENTED_EDGE('',*,*,#9199,.T.);
#12652=ORIENTED_EDGE('',*,*,#9209,.T.);
#12653=ORIENTED_EDGE('',*,*,#9206,.T.);
#12654=ORIENTED_EDGE('',*,*,#9203,.T.);
#12655=ORIENTED_EDGE('',*,*,#9211,.T.);
#12656=ORIENTED_EDGE('',*,*,#9212,.F.);
#12657=ORIENTED_EDGE('',*,*,#9213,.F.);
#12658=ORIENTED_EDGE('',*,*,#9214,.T.);
#12659=ORIENTED_EDGE('',*,*,#9215,.T.);
#12660=ORIENTED_EDGE('',*,*,#9214,.F.);
#12661=ORIENTED_EDGE('',*,*,#9216,.F.);
#12662=ORIENTED_EDGE('',*,*,#9217,.T.);
#12663=ORIENTED_EDGE('',*,*,#9218,.T.);
#12664=ORIENTED_EDGE('',*,*,#9217,.F.);
#12665=ORIENTED_EDGE('',*,*,#9219,.F.);
#12666=ORIENTED_EDGE('',*,*,#9220,.T.);
#12667=ORIENTED_EDGE('',*,*,#9221,.T.);
#12668=ORIENTED_EDGE('',*,*,#9220,.F.);
#12669=ORIENTED_EDGE('',*,*,#9222,.F.);
#12670=ORIENTED_EDGE('',*,*,#9212,.T.);
#12671=ORIENTED_EDGE('',*,*,#9213,.T.);
#12672=ORIENTED_EDGE('',*,*,#9222,.T.);
#12673=ORIENTED_EDGE('',*,*,#9219,.T.);
#12674=ORIENTED_EDGE('',*,*,#9216,.T.);
#12675=ORIENTED_EDGE('',*,*,#9211,.F.);
#12676=ORIENTED_EDGE('',*,*,#9215,.F.);
#12677=ORIENTED_EDGE('',*,*,#9218,.F.);
#12678=ORIENTED_EDGE('',*,*,#9221,.F.);
#12679=ORIENTED_EDGE('',*,*,#9223,.T.);
#12680=ORIENTED_EDGE('',*,*,#9224,.T.);
#12681=ORIENTED_EDGE('',*,*,#9225,.F.);
#12682=ORIENTED_EDGE('',*,*,#9224,.F.);
#12683=ORIENTED_EDGE('',*,*,#9226,.T.);
#12684=ORIENTED_EDGE('',*,*,#9227,.T.);
#12685=ORIENTED_EDGE('',*,*,#9228,.F.);
#12686=ORIENTED_EDGE('',*,*,#9227,.F.);
#12687=ORIENTED_EDGE('',*,*,#9229,.T.);
#12688=ORIENTED_EDGE('',*,*,#9230,.T.);
#12689=ORIENTED_EDGE('',*,*,#9231,.F.);
#12690=ORIENTED_EDGE('',*,*,#9230,.F.);
#12691=ORIENTED_EDGE('',*,*,#9232,.T.);
#12692=ORIENTED_EDGE('',*,*,#9233,.T.);
#12693=ORIENTED_EDGE('',*,*,#9234,.F.);
#12694=ORIENTED_EDGE('',*,*,#9233,.F.);
#12695=ORIENTED_EDGE('',*,*,#9235,.T.);
#12696=ORIENTED_EDGE('',*,*,#9236,.T.);
#12697=ORIENTED_EDGE('',*,*,#9237,.T.);
#12698=ORIENTED_EDGE('',*,*,#9238,.T.);
#12699=ORIENTED_EDGE('',*,*,#9232,.F.);
#12700=ORIENTED_EDGE('',*,*,#9229,.F.);
#12701=ORIENTED_EDGE('',*,*,#9226,.F.);
#12702=ORIENTED_EDGE('',*,*,#9223,.F.);
#12703=ORIENTED_EDGE('',*,*,#9239,.F.);
#12704=ORIENTED_EDGE('',*,*,#9240,.F.);
#12705=ORIENTED_EDGE('',*,*,#9241,.F.);
#12706=ORIENTED_EDGE('',*,*,#9242,.F.);
#12707=ORIENTED_EDGE('',*,*,#9231,.T.);
#12708=ORIENTED_EDGE('',*,*,#9225,.T.);
#12709=ORIENTED_EDGE('',*,*,#9228,.T.);
#12710=ORIENTED_EDGE('',*,*,#9234,.T.);
#12711=ORIENTED_EDGE('',*,*,#9239,.T.);
#12712=ORIENTED_EDGE('',*,*,#9243,.F.);
#12713=ORIENTED_EDGE('',*,*,#9235,.F.);
#12714=ORIENTED_EDGE('',*,*,#9244,.T.);
#12715=ORIENTED_EDGE('',*,*,#9242,.T.);
#12716=ORIENTED_EDGE('',*,*,#9245,.F.);
#12717=ORIENTED_EDGE('',*,*,#9236,.F.);
#12718=ORIENTED_EDGE('',*,*,#9243,.T.);
#12719=ORIENTED_EDGE('',*,*,#9241,.T.);
#12720=ORIENTED_EDGE('',*,*,#9246,.F.);
#12721=ORIENTED_EDGE('',*,*,#9237,.F.);
#12722=ORIENTED_EDGE('',*,*,#9245,.T.);
#12723=ORIENTED_EDGE('',*,*,#9240,.T.);
#12724=ORIENTED_EDGE('',*,*,#9244,.F.);
#12725=ORIENTED_EDGE('',*,*,#9238,.F.);
#12726=ORIENTED_EDGE('',*,*,#9246,.T.);
#12727=ORIENTED_EDGE('',*,*,#9247,.F.);
#12728=ORIENTED_EDGE('',*,*,#9248,.T.);
#12729=ORIENTED_EDGE('',*,*,#9249,.T.);
#12730=ORIENTED_EDGE('',*,*,#9248,.F.);
#12731=ORIENTED_EDGE('',*,*,#9250,.F.);
#12732=ORIENTED_EDGE('',*,*,#9251,.T.);
#12733=ORIENTED_EDGE('',*,*,#9252,.T.);
#12734=ORIENTED_EDGE('',*,*,#9251,.F.);
#12735=ORIENTED_EDGE('',*,*,#9253,.F.);
#12736=ORIENTED_EDGE('',*,*,#9254,.T.);
#12737=ORIENTED_EDGE('',*,*,#9255,.T.);
#12738=ORIENTED_EDGE('',*,*,#9254,.F.);
#12739=ORIENTED_EDGE('',*,*,#9256,.F.);
#12740=ORIENTED_EDGE('',*,*,#9257,.T.);
#12741=ORIENTED_EDGE('',*,*,#9258,.T.);
#12742=ORIENTED_EDGE('',*,*,#9257,.F.);
#12743=ORIENTED_EDGE('',*,*,#9259,.F.);
#12744=ORIENTED_EDGE('',*,*,#9260,.T.);
#12745=ORIENTED_EDGE('',*,*,#9261,.T.);
#12746=ORIENTED_EDGE('',*,*,#9260,.F.);
#12747=ORIENTED_EDGE('',*,*,#9262,.F.);
#12748=ORIENTED_EDGE('',*,*,#9263,.T.);
#12749=ORIENTED_EDGE('',*,*,#9264,.T.);
#12750=ORIENTED_EDGE('',*,*,#9263,.F.);
#12751=ORIENTED_EDGE('',*,*,#9265,.F.);
#12752=ORIENTED_EDGE('',*,*,#9266,.F.);
#12753=ORIENTED_EDGE('',*,*,#9267,.T.);
#12754=ORIENTED_EDGE('',*,*,#9268,.T.);
#12755=ORIENTED_EDGE('',*,*,#9269,.F.);
#12756=ORIENTED_EDGE('',*,*,#9270,.F.);
#12757=ORIENTED_EDGE('',*,*,#9271,.T.);
#12758=ORIENTED_EDGE('',*,*,#9266,.T.);
#12759=ORIENTED_EDGE('',*,*,#9272,.F.);
#12760=ORIENTED_EDGE('',*,*,#9273,.F.);
#12761=ORIENTED_EDGE('',*,*,#9274,.T.);
#12762=ORIENTED_EDGE('',*,*,#9270,.T.);
#12763=ORIENTED_EDGE('',*,*,#9275,.F.);
#12764=ORIENTED_EDGE('',*,*,#9268,.F.);
#12765=ORIENTED_EDGE('',*,*,#9276,.T.);
#12766=ORIENTED_EDGE('',*,*,#9273,.T.);
#12767=ORIENTED_EDGE('',*,*,#9267,.F.);
#12768=ORIENTED_EDGE('',*,*,#9271,.F.);
#12769=ORIENTED_EDGE('',*,*,#9274,.F.);
#12770=ORIENTED_EDGE('',*,*,#9276,.F.);
#12771=ORIENTED_EDGE('',*,*,#9247,.T.);
#12772=ORIENTED_EDGE('',*,*,#9250,.T.);
#12773=ORIENTED_EDGE('',*,*,#9253,.T.);
#12774=ORIENTED_EDGE('',*,*,#9256,.T.);
#12775=ORIENTED_EDGE('',*,*,#9259,.T.);
#12776=ORIENTED_EDGE('',*,*,#9262,.T.);
#12777=ORIENTED_EDGE('',*,*,#9265,.T.);
#12778=ORIENTED_EDGE('',*,*,#9275,.T.);
#12779=ORIENTED_EDGE('',*,*,#9272,.T.);
#12780=ORIENTED_EDGE('',*,*,#9269,.T.);
#12781=ORIENTED_EDGE('',*,*,#9249,.F.);
#12782=ORIENTED_EDGE('',*,*,#9252,.F.);
#12783=ORIENTED_EDGE('',*,*,#9255,.F.);
#12784=ORIENTED_EDGE('',*,*,#9258,.F.);
#12785=ORIENTED_EDGE('',*,*,#9261,.F.);
#12786=ORIENTED_EDGE('',*,*,#9264,.F.);
#12787=ORIENTED_EDGE('',*,*,#9277,.T.);
#12788=ORIENTED_EDGE('',*,*,#9278,.F.);
#12789=ORIENTED_EDGE('',*,*,#9279,.F.);
#12790=ORIENTED_EDGE('',*,*,#9280,.T.);
#12791=ORIENTED_EDGE('',*,*,#9281,.T.);
#12792=ORIENTED_EDGE('',*,*,#9282,.F.);
#12793=ORIENTED_EDGE('',*,*,#9283,.F.);
#12794=ORIENTED_EDGE('',*,*,#9278,.T.);
#12795=ORIENTED_EDGE('',*,*,#9284,.T.);
#12796=ORIENTED_EDGE('',*,*,#9285,.F.);
#12797=ORIENTED_EDGE('',*,*,#9286,.F.);
#12798=ORIENTED_EDGE('',*,*,#9282,.T.);
#12799=ORIENTED_EDGE('',*,*,#9287,.T.);
#12800=ORIENTED_EDGE('',*,*,#9288,.F.);
#12801=ORIENTED_EDGE('',*,*,#9289,.F.);
#12802=ORIENTED_EDGE('',*,*,#9285,.T.);
#12803=ORIENTED_EDGE('',*,*,#9290,.T.);
#12804=ORIENTED_EDGE('',*,*,#9291,.F.);
#12805=ORIENTED_EDGE('',*,*,#9292,.F.);
#12806=ORIENTED_EDGE('',*,*,#9288,.T.);
#12807=ORIENTED_EDGE('',*,*,#9293,.T.);
#12808=ORIENTED_EDGE('',*,*,#9294,.F.);
#12809=ORIENTED_EDGE('',*,*,#9295,.F.);
#12810=ORIENTED_EDGE('',*,*,#9291,.T.);
#12811=ORIENTED_EDGE('',*,*,#9296,.T.);
#12812=ORIENTED_EDGE('',*,*,#9280,.F.);
#12813=ORIENTED_EDGE('',*,*,#9297,.F.);
#12814=ORIENTED_EDGE('',*,*,#9294,.T.);
#12815=ORIENTED_EDGE('',*,*,#9279,.T.);
#12816=ORIENTED_EDGE('',*,*,#9283,.T.);
#12817=ORIENTED_EDGE('',*,*,#9286,.T.);
#12818=ORIENTED_EDGE('',*,*,#9289,.T.);
#12819=ORIENTED_EDGE('',*,*,#9292,.T.);
#12820=ORIENTED_EDGE('',*,*,#9295,.T.);
#12821=ORIENTED_EDGE('',*,*,#9297,.T.);
#12822=ORIENTED_EDGE('',*,*,#9277,.F.);
#12823=ORIENTED_EDGE('',*,*,#9296,.F.);
#12824=ORIENTED_EDGE('',*,*,#9293,.F.);
#12825=ORIENTED_EDGE('',*,*,#9290,.F.);
#12826=ORIENTED_EDGE('',*,*,#9287,.F.);
#12827=ORIENTED_EDGE('',*,*,#9284,.F.);
#12828=ORIENTED_EDGE('',*,*,#9281,.F.);
#12829=ORIENTED_EDGE('',*,*,#9298,.T.);
#12830=ORIENTED_EDGE('',*,*,#9299,.F.);
#12831=ORIENTED_EDGE('',*,*,#9300,.F.);
#12832=ORIENTED_EDGE('',*,*,#9301,.T.);
#12833=ORIENTED_EDGE('',*,*,#9302,.T.);
#12834=ORIENTED_EDGE('',*,*,#9303,.F.);
#12835=ORIENTED_EDGE('',*,*,#9304,.F.);
#12836=ORIENTED_EDGE('',*,*,#9299,.T.);
#12837=ORIENTED_EDGE('',*,*,#9305,.T.);
#12838=ORIENTED_EDGE('',*,*,#9306,.F.);
#12839=ORIENTED_EDGE('',*,*,#9307,.F.);
#12840=ORIENTED_EDGE('',*,*,#9303,.T.);
#12841=ORIENTED_EDGE('',*,*,#9308,.T.);
#12842=ORIENTED_EDGE('',*,*,#9309,.F.);
#12843=ORIENTED_EDGE('',*,*,#9310,.F.);
#12844=ORIENTED_EDGE('',*,*,#9306,.T.);
#12845=ORIENTED_EDGE('',*,*,#9311,.T.);
#12846=ORIENTED_EDGE('',*,*,#9312,.F.);
#12847=ORIENTED_EDGE('',*,*,#9313,.F.);
#12848=ORIENTED_EDGE('',*,*,#9309,.T.);
#12849=ORIENTED_EDGE('',*,*,#9314,.T.);
#12850=ORIENTED_EDGE('',*,*,#9315,.F.);
#12851=ORIENTED_EDGE('',*,*,#9316,.F.);
#12852=ORIENTED_EDGE('',*,*,#9312,.T.);
#12853=ORIENTED_EDGE('',*,*,#9317,.T.);
#12854=ORIENTED_EDGE('',*,*,#9301,.F.);
#12855=ORIENTED_EDGE('',*,*,#9318,.F.);
#12856=ORIENTED_EDGE('',*,*,#9315,.T.);
#12857=ORIENTED_EDGE('',*,*,#9300,.T.);
#12858=ORIENTED_EDGE('',*,*,#9304,.T.);
#12859=ORIENTED_EDGE('',*,*,#9307,.T.);
#12860=ORIENTED_EDGE('',*,*,#9310,.T.);
#12861=ORIENTED_EDGE('',*,*,#9313,.T.);
#12862=ORIENTED_EDGE('',*,*,#9316,.T.);
#12863=ORIENTED_EDGE('',*,*,#9318,.T.);
#12864=ORIENTED_EDGE('',*,*,#9298,.F.);
#12865=ORIENTED_EDGE('',*,*,#9317,.F.);
#12866=ORIENTED_EDGE('',*,*,#9314,.F.);
#12867=ORIENTED_EDGE('',*,*,#9311,.F.);
#12868=ORIENTED_EDGE('',*,*,#9308,.F.);
#12869=ORIENTED_EDGE('',*,*,#9305,.F.);
#12870=ORIENTED_EDGE('',*,*,#9302,.F.);
#12871=ORIENTED_EDGE('',*,*,#9319,.T.);
#12872=ORIENTED_EDGE('',*,*,#9320,.F.);
#12873=ORIENTED_EDGE('',*,*,#9321,.F.);
#12874=ORIENTED_EDGE('',*,*,#9322,.T.);
#12875=ORIENTED_EDGE('',*,*,#9323,.T.);
#12876=ORIENTED_EDGE('',*,*,#9324,.F.);
#12877=ORIENTED_EDGE('',*,*,#9325,.F.);
#12878=ORIENTED_EDGE('',*,*,#9320,.T.);
#12879=ORIENTED_EDGE('',*,*,#9326,.T.);
#12880=ORIENTED_EDGE('',*,*,#9327,.F.);
#12881=ORIENTED_EDGE('',*,*,#9328,.F.);
#12882=ORIENTED_EDGE('',*,*,#9324,.T.);
#12883=ORIENTED_EDGE('',*,*,#9329,.T.);
#12884=ORIENTED_EDGE('',*,*,#9330,.F.);
#12885=ORIENTED_EDGE('',*,*,#9331,.F.);
#12886=ORIENTED_EDGE('',*,*,#9327,.T.);
#12887=ORIENTED_EDGE('',*,*,#9332,.T.);
#12888=ORIENTED_EDGE('',*,*,#9333,.F.);
#12889=ORIENTED_EDGE('',*,*,#9334,.F.);
#12890=ORIENTED_EDGE('',*,*,#9330,.T.);
#12891=ORIENTED_EDGE('',*,*,#9335,.T.);
#12892=ORIENTED_EDGE('',*,*,#9336,.F.);
#12893=ORIENTED_EDGE('',*,*,#9337,.F.);
#12894=ORIENTED_EDGE('',*,*,#9333,.T.);
#12895=ORIENTED_EDGE('',*,*,#9338,.T.);
#12896=ORIENTED_EDGE('',*,*,#9322,.F.);
#12897=ORIENTED_EDGE('',*,*,#9339,.F.);
#12898=ORIENTED_EDGE('',*,*,#9336,.T.);
#12899=ORIENTED_EDGE('',*,*,#9321,.T.);
#12900=ORIENTED_EDGE('',*,*,#9325,.T.);
#12901=ORIENTED_EDGE('',*,*,#9328,.T.);
#12902=ORIENTED_EDGE('',*,*,#9331,.T.);
#12903=ORIENTED_EDGE('',*,*,#9334,.T.);
#12904=ORIENTED_EDGE('',*,*,#9337,.T.);
#12905=ORIENTED_EDGE('',*,*,#9339,.T.);
#12906=ORIENTED_EDGE('',*,*,#9319,.F.);
#12907=ORIENTED_EDGE('',*,*,#9338,.F.);
#12908=ORIENTED_EDGE('',*,*,#9335,.F.);
#12909=ORIENTED_EDGE('',*,*,#9332,.F.);
#12910=ORIENTED_EDGE('',*,*,#9329,.F.);
#12911=ORIENTED_EDGE('',*,*,#9326,.F.);
#12912=ORIENTED_EDGE('',*,*,#9323,.F.);
#12913=ORIENTED_EDGE('',*,*,#9340,.F.);
#12914=ORIENTED_EDGE('',*,*,#9341,.F.);
#12915=ORIENTED_EDGE('',*,*,#9342,.T.);
#12916=ORIENTED_EDGE('',*,*,#9343,.T.);
#12917=ORIENTED_EDGE('',*,*,#9344,.F.);
#12918=ORIENTED_EDGE('',*,*,#9345,.F.);
#12919=ORIENTED_EDGE('',*,*,#9346,.T.);
#12920=ORIENTED_EDGE('',*,*,#9341,.T.);
#12921=ORIENTED_EDGE('',*,*,#9347,.F.);
#12922=ORIENTED_EDGE('',*,*,#9348,.F.);
#12923=ORIENTED_EDGE('',*,*,#9349,.T.);
#12924=ORIENTED_EDGE('',*,*,#9345,.T.);
#12925=ORIENTED_EDGE('',*,*,#9350,.F.);
#12926=ORIENTED_EDGE('',*,*,#9351,.F.);
#12927=ORIENTED_EDGE('',*,*,#9352,.T.);
#12928=ORIENTED_EDGE('',*,*,#9348,.T.);
#12929=ORIENTED_EDGE('',*,*,#9353,.F.);
#12930=ORIENTED_EDGE('',*,*,#9354,.F.);
#12931=ORIENTED_EDGE('',*,*,#9355,.T.);
#12932=ORIENTED_EDGE('',*,*,#9351,.T.);
#12933=ORIENTED_EDGE('',*,*,#9356,.F.);
#12934=ORIENTED_EDGE('',*,*,#9357,.F.);
#12935=ORIENTED_EDGE('',*,*,#9358,.T.);
#12936=ORIENTED_EDGE('',*,*,#9354,.T.);
#12937=ORIENTED_EDGE('',*,*,#9359,.F.);
#12938=ORIENTED_EDGE('',*,*,#9343,.F.);
#12939=ORIENTED_EDGE('',*,*,#9360,.T.);
#12940=ORIENTED_EDGE('',*,*,#9357,.T.);
#12941=ORIENTED_EDGE('',*,*,#9342,.F.);
#12942=ORIENTED_EDGE('',*,*,#9346,.F.);
#12943=ORIENTED_EDGE('',*,*,#9349,.F.);
#12944=ORIENTED_EDGE('',*,*,#9352,.F.);
#12945=ORIENTED_EDGE('',*,*,#9355,.F.);
#12946=ORIENTED_EDGE('',*,*,#9358,.F.);
#12947=ORIENTED_EDGE('',*,*,#9360,.F.);
#12948=ORIENTED_EDGE('',*,*,#9340,.T.);
#12949=ORIENTED_EDGE('',*,*,#9359,.T.);
#12950=ORIENTED_EDGE('',*,*,#9356,.T.);
#12951=ORIENTED_EDGE('',*,*,#9353,.T.);
#12952=ORIENTED_EDGE('',*,*,#9350,.T.);
#12953=ORIENTED_EDGE('',*,*,#9347,.T.);
#12954=ORIENTED_EDGE('',*,*,#9344,.T.);
#12955=ORIENTED_EDGE('',*,*,#9361,.F.);
#12956=ORIENTED_EDGE('',*,*,#9362,.F.);
#12957=ORIENTED_EDGE('',*,*,#9363,.T.);
#12958=ORIENTED_EDGE('',*,*,#9364,.T.);
#12959=ORIENTED_EDGE('',*,*,#9365,.F.);
#12960=ORIENTED_EDGE('',*,*,#9366,.F.);
#12961=ORIENTED_EDGE('',*,*,#9367,.T.);
#12962=ORIENTED_EDGE('',*,*,#9362,.T.);
#12963=ORIENTED_EDGE('',*,*,#9368,.F.);
#12964=ORIENTED_EDGE('',*,*,#9369,.F.);
#12965=ORIENTED_EDGE('',*,*,#9370,.T.);
#12966=ORIENTED_EDGE('',*,*,#9366,.T.);
#12967=ORIENTED_EDGE('',*,*,#9371,.F.);
#12968=ORIENTED_EDGE('',*,*,#9372,.F.);
#12969=ORIENTED_EDGE('',*,*,#9373,.T.);
#12970=ORIENTED_EDGE('',*,*,#9369,.T.);
#12971=ORIENTED_EDGE('',*,*,#9374,.F.);
#12972=ORIENTED_EDGE('',*,*,#9375,.F.);
#12973=ORIENTED_EDGE('',*,*,#9376,.T.);
#12974=ORIENTED_EDGE('',*,*,#9372,.T.);
#12975=ORIENTED_EDGE('',*,*,#9377,.F.);
#12976=ORIENTED_EDGE('',*,*,#9378,.F.);
#12977=ORIENTED_EDGE('',*,*,#9379,.T.);
#12978=ORIENTED_EDGE('',*,*,#9375,.T.);
#12979=ORIENTED_EDGE('',*,*,#9380,.F.);
#12980=ORIENTED_EDGE('',*,*,#9364,.F.);
#12981=ORIENTED_EDGE('',*,*,#9381,.T.);
#12982=ORIENTED_EDGE('',*,*,#9378,.T.);
#12983=ORIENTED_EDGE('',*,*,#9363,.F.);
#12984=ORIENTED_EDGE('',*,*,#9367,.F.);
#12985=ORIENTED_EDGE('',*,*,#9370,.F.);
#12986=ORIENTED_EDGE('',*,*,#9373,.F.);
#12987=ORIENTED_EDGE('',*,*,#9376,.F.);
#12988=ORIENTED_EDGE('',*,*,#9379,.F.);
#12989=ORIENTED_EDGE('',*,*,#9381,.F.);
#12990=ORIENTED_EDGE('',*,*,#9361,.T.);
#12991=ORIENTED_EDGE('',*,*,#9380,.T.);
#12992=ORIENTED_EDGE('',*,*,#9377,.T.);
#12993=ORIENTED_EDGE('',*,*,#9374,.T.);
#12994=ORIENTED_EDGE('',*,*,#9371,.T.);
#12995=ORIENTED_EDGE('',*,*,#9368,.T.);
#12996=ORIENTED_EDGE('',*,*,#9365,.T.);
#12997=ORIENTED_EDGE('',*,*,#9382,.F.);
#12998=ORIENTED_EDGE('',*,*,#9383,.F.);
#12999=ORIENTED_EDGE('',*,*,#9384,.T.);
#13000=ORIENTED_EDGE('',*,*,#9385,.T.);
#13001=ORIENTED_EDGE('',*,*,#9386,.F.);
#13002=ORIENTED_EDGE('',*,*,#9387,.F.);
#13003=ORIENTED_EDGE('',*,*,#9388,.T.);
#13004=ORIENTED_EDGE('',*,*,#9383,.T.);
#13005=ORIENTED_EDGE('',*,*,#9389,.F.);
#13006=ORIENTED_EDGE('',*,*,#9390,.F.);
#13007=ORIENTED_EDGE('',*,*,#9391,.T.);
#13008=ORIENTED_EDGE('',*,*,#9387,.T.);
#13009=ORIENTED_EDGE('',*,*,#9392,.F.);
#13010=ORIENTED_EDGE('',*,*,#9393,.F.);
#13011=ORIENTED_EDGE('',*,*,#9394,.T.);
#13012=ORIENTED_EDGE('',*,*,#9390,.T.);
#13013=ORIENTED_EDGE('',*,*,#9395,.F.);
#13014=ORIENTED_EDGE('',*,*,#9396,.F.);
#13015=ORIENTED_EDGE('',*,*,#9397,.T.);
#13016=ORIENTED_EDGE('',*,*,#9393,.T.);
#13017=ORIENTED_EDGE('',*,*,#9398,.F.);
#13018=ORIENTED_EDGE('',*,*,#9399,.F.);
#13019=ORIENTED_EDGE('',*,*,#9400,.T.);
#13020=ORIENTED_EDGE('',*,*,#9396,.T.);
#13021=ORIENTED_EDGE('',*,*,#9401,.F.);
#13022=ORIENTED_EDGE('',*,*,#9385,.F.);
#13023=ORIENTED_EDGE('',*,*,#9402,.T.);
#13024=ORIENTED_EDGE('',*,*,#9399,.T.);
#13025=ORIENTED_EDGE('',*,*,#9384,.F.);
#13026=ORIENTED_EDGE('',*,*,#9388,.F.);
#13027=ORIENTED_EDGE('',*,*,#9391,.F.);
#13028=ORIENTED_EDGE('',*,*,#9394,.F.);
#13029=ORIENTED_EDGE('',*,*,#9397,.F.);
#13030=ORIENTED_EDGE('',*,*,#9400,.F.);
#13031=ORIENTED_EDGE('',*,*,#9402,.F.);
#13032=ORIENTED_EDGE('',*,*,#9382,.T.);
#13033=ORIENTED_EDGE('',*,*,#9401,.T.);
#13034=ORIENTED_EDGE('',*,*,#9398,.T.);
#13035=ORIENTED_EDGE('',*,*,#9395,.T.);
#13036=ORIENTED_EDGE('',*,*,#9392,.T.);
#13037=ORIENTED_EDGE('',*,*,#9389,.T.);
#13038=ORIENTED_EDGE('',*,*,#9386,.T.);
#13039=ORIENTED_EDGE('',*,*,#9403,.T.);
#13040=ORIENTED_EDGE('',*,*,#9404,.F.);
#13041=ORIENTED_EDGE('',*,*,#9405,.F.);
#13042=ORIENTED_EDGE('',*,*,#9406,.T.);
#13043=ORIENTED_EDGE('',*,*,#9407,.T.);
#13044=ORIENTED_EDGE('',*,*,#9406,.F.);
#13045=ORIENTED_EDGE('',*,*,#9408,.F.);
#13046=ORIENTED_EDGE('',*,*,#9409,.T.);
#13047=ORIENTED_EDGE('',*,*,#9410,.T.);
#13048=ORIENTED_EDGE('',*,*,#9409,.F.);
#13049=ORIENTED_EDGE('',*,*,#9411,.F.);
#13050=ORIENTED_EDGE('',*,*,#9412,.T.);
#13051=ORIENTED_EDGE('',*,*,#9413,.T.);
#13052=ORIENTED_EDGE('',*,*,#9412,.F.);
#13053=ORIENTED_EDGE('',*,*,#9414,.F.);
#13054=ORIENTED_EDGE('',*,*,#9415,.T.);
#13055=ORIENTED_EDGE('',*,*,#9416,.T.);
#13056=ORIENTED_EDGE('',*,*,#9415,.F.);
#13057=ORIENTED_EDGE('',*,*,#9417,.F.);
#13058=ORIENTED_EDGE('',*,*,#9418,.T.);
#13059=ORIENTED_EDGE('',*,*,#9419,.T.);
#13060=ORIENTED_EDGE('',*,*,#9418,.F.);
#13061=ORIENTED_EDGE('',*,*,#9420,.F.);
#13062=ORIENTED_EDGE('',*,*,#9421,.T.);
#13063=ORIENTED_EDGE('',*,*,#9422,.T.);
#13064=ORIENTED_EDGE('',*,*,#9421,.F.);
#13065=ORIENTED_EDGE('',*,*,#9423,.F.);
#13066=ORIENTED_EDGE('',*,*,#9404,.T.);
#13067=ORIENTED_EDGE('',*,*,#9405,.T.);
#13068=ORIENTED_EDGE('',*,*,#9423,.T.);
#13069=ORIENTED_EDGE('',*,*,#9420,.T.);
#13070=ORIENTED_EDGE('',*,*,#9417,.T.);
#13071=ORIENTED_EDGE('',*,*,#9414,.T.);
#13072=ORIENTED_EDGE('',*,*,#9411,.T.);
#13073=ORIENTED_EDGE('',*,*,#9408,.T.);
#13074=ORIENTED_EDGE('',*,*,#9403,.F.);
#13075=ORIENTED_EDGE('',*,*,#9407,.F.);
#13076=ORIENTED_EDGE('',*,*,#9410,.F.);
#13077=ORIENTED_EDGE('',*,*,#9413,.F.);
#13078=ORIENTED_EDGE('',*,*,#9416,.F.);
#13079=ORIENTED_EDGE('',*,*,#9419,.F.);
#13080=ORIENTED_EDGE('',*,*,#9422,.F.);
#13081=ORIENTED_EDGE('',*,*,#9424,.T.);
#13082=ORIENTED_EDGE('',*,*,#9425,.F.);
#13083=ORIENTED_EDGE('',*,*,#9426,.F.);
#13084=ORIENTED_EDGE('',*,*,#9427,.T.);
#13085=ORIENTED_EDGE('',*,*,#9428,.T.);
#13086=ORIENTED_EDGE('',*,*,#9427,.F.);
#13087=ORIENTED_EDGE('',*,*,#9429,.F.);
#13088=ORIENTED_EDGE('',*,*,#9430,.T.);
#13089=ORIENTED_EDGE('',*,*,#9431,.T.);
#13090=ORIENTED_EDGE('',*,*,#9430,.F.);
#13091=ORIENTED_EDGE('',*,*,#9432,.F.);
#13092=ORIENTED_EDGE('',*,*,#9433,.T.);
#13093=ORIENTED_EDGE('',*,*,#9434,.T.);
#13094=ORIENTED_EDGE('',*,*,#9433,.F.);
#13095=ORIENTED_EDGE('',*,*,#9435,.F.);
#13096=ORIENTED_EDGE('',*,*,#9436,.T.);
#13097=ORIENTED_EDGE('',*,*,#9437,.T.);
#13098=ORIENTED_EDGE('',*,*,#9436,.F.);
#13099=ORIENTED_EDGE('',*,*,#9438,.F.);
#13100=ORIENTED_EDGE('',*,*,#9439,.T.);
#13101=ORIENTED_EDGE('',*,*,#9440,.T.);
#13102=ORIENTED_EDGE('',*,*,#9439,.F.);
#13103=ORIENTED_EDGE('',*,*,#9441,.F.);
#13104=ORIENTED_EDGE('',*,*,#9442,.T.);
#13105=ORIENTED_EDGE('',*,*,#9443,.T.);
#13106=ORIENTED_EDGE('',*,*,#9442,.F.);
#13107=ORIENTED_EDGE('',*,*,#9444,.F.);
#13108=ORIENTED_EDGE('',*,*,#9425,.T.);
#13109=ORIENTED_EDGE('',*,*,#9426,.T.);
#13110=ORIENTED_EDGE('',*,*,#9444,.T.);
#13111=ORIENTED_EDGE('',*,*,#9441,.T.);
#13112=ORIENTED_EDGE('',*,*,#9438,.T.);
#13113=ORIENTED_EDGE('',*,*,#9435,.T.);
#13114=ORIENTED_EDGE('',*,*,#9432,.T.);
#13115=ORIENTED_EDGE('',*,*,#9429,.T.);
#13116=ORIENTED_EDGE('',*,*,#9424,.F.);
#13117=ORIENTED_EDGE('',*,*,#9428,.F.);
#13118=ORIENTED_EDGE('',*,*,#9431,.F.);
#13119=ORIENTED_EDGE('',*,*,#9434,.F.);
#13120=ORIENTED_EDGE('',*,*,#9437,.F.);
#13121=ORIENTED_EDGE('',*,*,#9440,.F.);
#13122=ORIENTED_EDGE('',*,*,#9443,.F.);
#13123=ORIENTED_EDGE('',*,*,#9445,.F.);
#13124=ORIENTED_EDGE('',*,*,#9446,.F.);
#13125=ORIENTED_EDGE('',*,*,#9447,.T.);
#13126=ORIENTED_EDGE('',*,*,#9448,.T.);
#13127=ORIENTED_EDGE('',*,*,#9449,.F.);
#13128=ORIENTED_EDGE('',*,*,#9448,.F.);
#13129=ORIENTED_EDGE('',*,*,#9450,.T.);
#13130=ORIENTED_EDGE('',*,*,#9451,.T.);
#13131=ORIENTED_EDGE('',*,*,#9452,.F.);
#13132=ORIENTED_EDGE('',*,*,#9451,.F.);
#13133=ORIENTED_EDGE('',*,*,#9453,.T.);
#13134=ORIENTED_EDGE('',*,*,#9454,.T.);
#13135=ORIENTED_EDGE('',*,*,#9455,.F.);
#13136=ORIENTED_EDGE('',*,*,#9454,.F.);
#13137=ORIENTED_EDGE('',*,*,#9456,.T.);
#13138=ORIENTED_EDGE('',*,*,#9457,.T.);
#13139=ORIENTED_EDGE('',*,*,#9458,.F.);
#13140=ORIENTED_EDGE('',*,*,#9457,.F.);
#13141=ORIENTED_EDGE('',*,*,#9459,.T.);
#13142=ORIENTED_EDGE('',*,*,#9460,.T.);
#13143=ORIENTED_EDGE('',*,*,#9461,.F.);
#13144=ORIENTED_EDGE('',*,*,#9460,.F.);
#13145=ORIENTED_EDGE('',*,*,#9462,.T.);
#13146=ORIENTED_EDGE('',*,*,#9463,.T.);
#13147=ORIENTED_EDGE('',*,*,#9464,.F.);
#13148=ORIENTED_EDGE('',*,*,#9463,.F.);
#13149=ORIENTED_EDGE('',*,*,#9465,.T.);
#13150=ORIENTED_EDGE('',*,*,#9446,.T.);
#13151=ORIENTED_EDGE('',*,*,#9447,.F.);
#13152=ORIENTED_EDGE('',*,*,#9465,.F.);
#13153=ORIENTED_EDGE('',*,*,#9462,.F.);
#13154=ORIENTED_EDGE('',*,*,#9459,.F.);
#13155=ORIENTED_EDGE('',*,*,#9456,.F.);
#13156=ORIENTED_EDGE('',*,*,#9453,.F.);
#13157=ORIENTED_EDGE('',*,*,#9450,.F.);
#13158=ORIENTED_EDGE('',*,*,#9445,.T.);
#13159=ORIENTED_EDGE('',*,*,#9449,.T.);
#13160=ORIENTED_EDGE('',*,*,#9452,.T.);
#13161=ORIENTED_EDGE('',*,*,#9455,.T.);
#13162=ORIENTED_EDGE('',*,*,#9458,.T.);
#13163=ORIENTED_EDGE('',*,*,#9461,.T.);
#13164=ORIENTED_EDGE('',*,*,#9464,.T.);
#13165=ORIENTED_EDGE('',*,*,#9466,.F.);
#13166=ORIENTED_EDGE('',*,*,#9467,.F.);
#13167=ORIENTED_EDGE('',*,*,#9468,.T.);
#13168=ORIENTED_EDGE('',*,*,#9469,.T.);
#13169=ORIENTED_EDGE('',*,*,#9470,.F.);
#13170=ORIENTED_EDGE('',*,*,#9469,.F.);
#13171=ORIENTED_EDGE('',*,*,#9471,.T.);
#13172=ORIENTED_EDGE('',*,*,#9472,.T.);
#13173=ORIENTED_EDGE('',*,*,#9473,.F.);
#13174=ORIENTED_EDGE('',*,*,#9472,.F.);
#13175=ORIENTED_EDGE('',*,*,#9474,.T.);
#13176=ORIENTED_EDGE('',*,*,#9475,.T.);
#13177=ORIENTED_EDGE('',*,*,#9476,.F.);
#13178=ORIENTED_EDGE('',*,*,#9475,.F.);
#13179=ORIENTED_EDGE('',*,*,#9477,.T.);
#13180=ORIENTED_EDGE('',*,*,#9478,.T.);
#13181=ORIENTED_EDGE('',*,*,#9479,.F.);
#13182=ORIENTED_EDGE('',*,*,#9478,.F.);
#13183=ORIENTED_EDGE('',*,*,#9480,.T.);
#13184=ORIENTED_EDGE('',*,*,#9481,.T.);
#13185=ORIENTED_EDGE('',*,*,#9482,.F.);
#13186=ORIENTED_EDGE('',*,*,#9481,.F.);
#13187=ORIENTED_EDGE('',*,*,#9483,.T.);
#13188=ORIENTED_EDGE('',*,*,#9484,.T.);
#13189=ORIENTED_EDGE('',*,*,#9485,.F.);
#13190=ORIENTED_EDGE('',*,*,#9484,.F.);
#13191=ORIENTED_EDGE('',*,*,#9486,.T.);
#13192=ORIENTED_EDGE('',*,*,#9467,.T.);
#13193=ORIENTED_EDGE('',*,*,#9468,.F.);
#13194=ORIENTED_EDGE('',*,*,#9486,.F.);
#13195=ORIENTED_EDGE('',*,*,#9483,.F.);
#13196=ORIENTED_EDGE('',*,*,#9480,.F.);
#13197=ORIENTED_EDGE('',*,*,#9477,.F.);
#13198=ORIENTED_EDGE('',*,*,#9474,.F.);
#13199=ORIENTED_EDGE('',*,*,#9471,.F.);
#13200=ORIENTED_EDGE('',*,*,#9466,.T.);
#13201=ORIENTED_EDGE('',*,*,#9470,.T.);
#13202=ORIENTED_EDGE('',*,*,#9473,.T.);
#13203=ORIENTED_EDGE('',*,*,#9476,.T.);
#13204=ORIENTED_EDGE('',*,*,#9479,.T.);
#13205=ORIENTED_EDGE('',*,*,#9482,.T.);
#13206=ORIENTED_EDGE('',*,*,#9485,.T.);
#13207=ORIENTED_EDGE('',*,*,#9487,.F.);
#13208=ORIENTED_EDGE('',*,*,#9488,.F.);
#13209=ORIENTED_EDGE('',*,*,#9489,.T.);
#13210=ORIENTED_EDGE('',*,*,#9490,.T.);
#13211=ORIENTED_EDGE('',*,*,#9491,.F.);
#13212=ORIENTED_EDGE('',*,*,#9490,.F.);
#13213=ORIENTED_EDGE('',*,*,#9492,.T.);
#13214=ORIENTED_EDGE('',*,*,#9493,.T.);
#13215=ORIENTED_EDGE('',*,*,#9494,.F.);
#13216=ORIENTED_EDGE('',*,*,#9493,.F.);
#13217=ORIENTED_EDGE('',*,*,#9495,.T.);
#13218=ORIENTED_EDGE('',*,*,#9496,.T.);
#13219=ORIENTED_EDGE('',*,*,#9497,.F.);
#13220=ORIENTED_EDGE('',*,*,#9496,.F.);
#13221=ORIENTED_EDGE('',*,*,#9498,.T.);
#13222=ORIENTED_EDGE('',*,*,#9499,.T.);
#13223=ORIENTED_EDGE('',*,*,#9500,.F.);
#13224=ORIENTED_EDGE('',*,*,#9499,.F.);
#13225=ORIENTED_EDGE('',*,*,#9501,.T.);
#13226=ORIENTED_EDGE('',*,*,#9502,.T.);
#13227=ORIENTED_EDGE('',*,*,#9503,.F.);
#13228=ORIENTED_EDGE('',*,*,#9502,.F.);
#13229=ORIENTED_EDGE('',*,*,#9504,.T.);
#13230=ORIENTED_EDGE('',*,*,#9505,.T.);
#13231=ORIENTED_EDGE('',*,*,#9506,.F.);
#13232=ORIENTED_EDGE('',*,*,#9505,.F.);
#13233=ORIENTED_EDGE('',*,*,#9507,.T.);
#13234=ORIENTED_EDGE('',*,*,#9488,.T.);
#13235=ORIENTED_EDGE('',*,*,#9489,.F.);
#13236=ORIENTED_EDGE('',*,*,#9507,.F.);
#13237=ORIENTED_EDGE('',*,*,#9504,.F.);
#13238=ORIENTED_EDGE('',*,*,#9501,.F.);
#13239=ORIENTED_EDGE('',*,*,#9498,.F.);
#13240=ORIENTED_EDGE('',*,*,#9495,.F.);
#13241=ORIENTED_EDGE('',*,*,#9492,.F.);
#13242=ORIENTED_EDGE('',*,*,#9487,.T.);
#13243=ORIENTED_EDGE('',*,*,#9491,.T.);
#13244=ORIENTED_EDGE('',*,*,#9494,.T.);
#13245=ORIENTED_EDGE('',*,*,#9497,.T.);
#13246=ORIENTED_EDGE('',*,*,#9500,.T.);
#13247=ORIENTED_EDGE('',*,*,#9503,.T.);
#13248=ORIENTED_EDGE('',*,*,#9506,.T.);
#13249=ORIENTED_EDGE('',*,*,#9508,.F.);
#13250=ORIENTED_EDGE('',*,*,#9509,.T.);
#13251=ORIENTED_EDGE('',*,*,#9510,.T.);
#13252=ORIENTED_EDGE('',*,*,#9509,.F.);
#13253=ORIENTED_EDGE('',*,*,#9511,.F.);
#13254=ORIENTED_EDGE('',*,*,#9512,.T.);
#13255=ORIENTED_EDGE('',*,*,#9513,.T.);
#13256=ORIENTED_EDGE('',*,*,#9512,.F.);
#13257=ORIENTED_EDGE('',*,*,#9514,.F.);
#13258=ORIENTED_EDGE('',*,*,#9515,.T.);
#13259=ORIENTED_EDGE('',*,*,#9516,.T.);
#13260=ORIENTED_EDGE('',*,*,#9515,.F.);
#13261=ORIENTED_EDGE('',*,*,#9517,.F.);
#13262=ORIENTED_EDGE('',*,*,#9518,.T.);
#13263=ORIENTED_EDGE('',*,*,#9519,.T.);
#13264=ORIENTED_EDGE('',*,*,#9518,.F.);
#13265=ORIENTED_EDGE('',*,*,#9520,.F.);
#13266=ORIENTED_EDGE('',*,*,#9521,.F.);
#13267=ORIENTED_EDGE('',*,*,#9522,.F.);
#13268=ORIENTED_EDGE('',*,*,#9523,.F.);
#13269=ORIENTED_EDGE('',*,*,#9517,.T.);
#13270=ORIENTED_EDGE('',*,*,#9514,.T.);
#13271=ORIENTED_EDGE('',*,*,#9511,.T.);
#13272=ORIENTED_EDGE('',*,*,#9508,.T.);
#13273=ORIENTED_EDGE('',*,*,#9524,.T.);
#13274=ORIENTED_EDGE('',*,*,#9525,.T.);
#13275=ORIENTED_EDGE('',*,*,#9526,.T.);
#13276=ORIENTED_EDGE('',*,*,#9527,.T.);
#13277=ORIENTED_EDGE('',*,*,#9516,.F.);
#13278=ORIENTED_EDGE('',*,*,#9510,.F.);
#13279=ORIENTED_EDGE('',*,*,#9513,.F.);
#13280=ORIENTED_EDGE('',*,*,#9519,.F.);
#13281=ORIENTED_EDGE('',*,*,#9524,.F.);
#13282=ORIENTED_EDGE('',*,*,#9528,.F.);
#13283=ORIENTED_EDGE('',*,*,#9520,.T.);
#13284=ORIENTED_EDGE('',*,*,#9529,.T.);
#13285=ORIENTED_EDGE('',*,*,#9525,.F.);
#13286=ORIENTED_EDGE('',*,*,#9529,.F.);
#13287=ORIENTED_EDGE('',*,*,#9523,.T.);
#13288=ORIENTED_EDGE('',*,*,#9530,.T.);
#13289=ORIENTED_EDGE('',*,*,#9526,.F.);
#13290=ORIENTED_EDGE('',*,*,#9530,.F.);
#13291=ORIENTED_EDGE('',*,*,#9522,.T.);
#13292=ORIENTED_EDGE('',*,*,#9531,.T.);
#13293=ORIENTED_EDGE('',*,*,#9527,.F.);
#13294=ORIENTED_EDGE('',*,*,#9531,.F.);
#13295=ORIENTED_EDGE('',*,*,#9521,.T.);
#13296=ORIENTED_EDGE('',*,*,#9528,.T.);
#13297=ORIENTED_EDGE('',*,*,#9532,.T.);
#13298=ORIENTED_EDGE('',*,*,#9533,.F.);
#13299=ORIENTED_EDGE('',*,*,#9534,.F.);
#13300=ORIENTED_EDGE('',*,*,#9535,.T.);
#13301=ORIENTED_EDGE('',*,*,#9536,.T.);
#13302=ORIENTED_EDGE('',*,*,#9537,.F.);
#13303=ORIENTED_EDGE('',*,*,#9538,.F.);
#13304=ORIENTED_EDGE('',*,*,#9533,.T.);
#13305=ORIENTED_EDGE('',*,*,#9539,.T.);
#13306=ORIENTED_EDGE('',*,*,#9540,.F.);
#13307=ORIENTED_EDGE('',*,*,#9541,.F.);
#13308=ORIENTED_EDGE('',*,*,#9537,.T.);
#13309=ORIENTED_EDGE('',*,*,#9542,.T.);
#13310=ORIENTED_EDGE('',*,*,#9535,.F.);
#13311=ORIENTED_EDGE('',*,*,#9543,.F.);
#13312=ORIENTED_EDGE('',*,*,#9540,.T.);
#13313=ORIENTED_EDGE('',*,*,#9534,.T.);
#13314=ORIENTED_EDGE('',*,*,#9538,.T.);
#13315=ORIENTED_EDGE('',*,*,#9541,.T.);
#13316=ORIENTED_EDGE('',*,*,#9543,.T.);
#13317=ORIENTED_EDGE('',*,*,#9532,.F.);
#13318=ORIENTED_EDGE('',*,*,#9542,.F.);
#13319=ORIENTED_EDGE('',*,*,#9539,.F.);
#13320=ORIENTED_EDGE('',*,*,#9536,.F.);
#13321=ORIENTED_EDGE('',*,*,#9544,.T.);
#13322=ORIENTED_EDGE('',*,*,#9545,.F.);
#13323=ORIENTED_EDGE('',*,*,#9546,.F.);
#13324=ORIENTED_EDGE('',*,*,#9547,.T.);
#13325=ORIENTED_EDGE('',*,*,#9548,.T.);
#13326=ORIENTED_EDGE('',*,*,#9549,.F.);
#13327=ORIENTED_EDGE('',*,*,#9550,.F.);
#13328=ORIENTED_EDGE('',*,*,#9545,.T.);
#13329=ORIENTED_EDGE('',*,*,#9551,.T.);
#13330=ORIENTED_EDGE('',*,*,#9552,.F.);
#13331=ORIENTED_EDGE('',*,*,#9553,.F.);
#13332=ORIENTED_EDGE('',*,*,#9549,.T.);
#13333=ORIENTED_EDGE('',*,*,#9554,.T.);
#13334=ORIENTED_EDGE('',*,*,#9547,.F.);
#13335=ORIENTED_EDGE('',*,*,#9555,.F.);
#13336=ORIENTED_EDGE('',*,*,#9552,.T.);
#13337=ORIENTED_EDGE('',*,*,#9546,.T.);
#13338=ORIENTED_EDGE('',*,*,#9550,.T.);
#13339=ORIENTED_EDGE('',*,*,#9553,.T.);
#13340=ORIENTED_EDGE('',*,*,#9555,.T.);
#13341=ORIENTED_EDGE('',*,*,#9544,.F.);
#13342=ORIENTED_EDGE('',*,*,#9554,.F.);
#13343=ORIENTED_EDGE('',*,*,#9551,.F.);
#13344=ORIENTED_EDGE('',*,*,#9548,.F.);
#13345=ORIENTED_EDGE('',*,*,#9556,.T.);
#13346=ORIENTED_EDGE('',*,*,#9557,.F.);
#13347=ORIENTED_EDGE('',*,*,#9558,.F.);
#13348=ORIENTED_EDGE('',*,*,#9559,.T.);
#13349=ORIENTED_EDGE('',*,*,#9560,.T.);
#13350=ORIENTED_EDGE('',*,*,#9561,.F.);
#13351=ORIENTED_EDGE('',*,*,#9562,.F.);
#13352=ORIENTED_EDGE('',*,*,#9557,.T.);
#13353=ORIENTED_EDGE('',*,*,#9563,.T.);
#13354=ORIENTED_EDGE('',*,*,#9564,.F.);
#13355=ORIENTED_EDGE('',*,*,#9565,.F.);
#13356=ORIENTED_EDGE('',*,*,#9561,.T.);
#13357=ORIENTED_EDGE('',*,*,#9566,.T.);
#13358=ORIENTED_EDGE('',*,*,#9559,.F.);
#13359=ORIENTED_EDGE('',*,*,#9567,.F.);
#13360=ORIENTED_EDGE('',*,*,#9564,.T.);
#13361=ORIENTED_EDGE('',*,*,#9558,.T.);
#13362=ORIENTED_EDGE('',*,*,#9562,.T.);
#13363=ORIENTED_EDGE('',*,*,#9565,.T.);
#13364=ORIENTED_EDGE('',*,*,#9567,.T.);
#13365=ORIENTED_EDGE('',*,*,#9556,.F.);
#13366=ORIENTED_EDGE('',*,*,#9566,.F.);
#13367=ORIENTED_EDGE('',*,*,#9563,.F.);
#13368=ORIENTED_EDGE('',*,*,#9560,.F.);
#13369=ORIENTED_EDGE('',*,*,#9568,.T.);
#13370=ORIENTED_EDGE('',*,*,#9569,.F.);
#13371=ORIENTED_EDGE('',*,*,#9570,.F.);
#13372=ORIENTED_EDGE('',*,*,#9571,.T.);
#13373=ORIENTED_EDGE('',*,*,#9572,.T.);
#13374=ORIENTED_EDGE('',*,*,#9573,.F.);
#13375=ORIENTED_EDGE('',*,*,#9574,.F.);
#13376=ORIENTED_EDGE('',*,*,#9569,.T.);
#13377=ORIENTED_EDGE('',*,*,#9575,.T.);
#13378=ORIENTED_EDGE('',*,*,#9576,.F.);
#13379=ORIENTED_EDGE('',*,*,#9577,.F.);
#13380=ORIENTED_EDGE('',*,*,#9573,.T.);
#13381=ORIENTED_EDGE('',*,*,#9578,.T.);
#13382=ORIENTED_EDGE('',*,*,#9571,.F.);
#13383=ORIENTED_EDGE('',*,*,#9579,.F.);
#13384=ORIENTED_EDGE('',*,*,#9576,.T.);
#13385=ORIENTED_EDGE('',*,*,#9570,.T.);
#13386=ORIENTED_EDGE('',*,*,#9574,.T.);
#13387=ORIENTED_EDGE('',*,*,#9577,.T.);
#13388=ORIENTED_EDGE('',*,*,#9579,.T.);
#13389=ORIENTED_EDGE('',*,*,#9568,.F.);
#13390=ORIENTED_EDGE('',*,*,#9578,.F.);
#13391=ORIENTED_EDGE('',*,*,#9575,.F.);
#13392=ORIENTED_EDGE('',*,*,#9572,.F.);
#13393=ORIENTED_EDGE('',*,*,#9580,.T.);
#13394=ORIENTED_EDGE('',*,*,#9581,.F.);
#13395=ORIENTED_EDGE('',*,*,#9582,.F.);
#13396=ORIENTED_EDGE('',*,*,#9583,.T.);
#13397=ORIENTED_EDGE('',*,*,#9584,.T.);
#13398=ORIENTED_EDGE('',*,*,#9585,.F.);
#13399=ORIENTED_EDGE('',*,*,#9586,.F.);
#13400=ORIENTED_EDGE('',*,*,#9581,.T.);
#13401=ORIENTED_EDGE('',*,*,#9587,.T.);
#13402=ORIENTED_EDGE('',*,*,#9588,.F.);
#13403=ORIENTED_EDGE('',*,*,#9589,.F.);
#13404=ORIENTED_EDGE('',*,*,#9585,.T.);
#13405=ORIENTED_EDGE('',*,*,#9590,.T.);
#13406=ORIENTED_EDGE('',*,*,#9583,.F.);
#13407=ORIENTED_EDGE('',*,*,#9591,.F.);
#13408=ORIENTED_EDGE('',*,*,#9588,.T.);
#13409=ORIENTED_EDGE('',*,*,#9582,.T.);
#13410=ORIENTED_EDGE('',*,*,#9586,.T.);
#13411=ORIENTED_EDGE('',*,*,#9589,.T.);
#13412=ORIENTED_EDGE('',*,*,#9591,.T.);
#13413=ORIENTED_EDGE('',*,*,#9580,.F.);
#13414=ORIENTED_EDGE('',*,*,#9590,.F.);
#13415=ORIENTED_EDGE('',*,*,#9587,.F.);
#13416=ORIENTED_EDGE('',*,*,#9584,.F.);
#13417=ORIENTED_EDGE('',*,*,#9592,.T.);
#13418=ORIENTED_EDGE('',*,*,#9593,.F.);
#13419=ORIENTED_EDGE('',*,*,#9594,.F.);
#13420=ORIENTED_EDGE('',*,*,#9595,.T.);
#13421=ORIENTED_EDGE('',*,*,#9596,.T.);
#13422=ORIENTED_EDGE('',*,*,#9597,.F.);
#13423=ORIENTED_EDGE('',*,*,#9598,.F.);
#13424=ORIENTED_EDGE('',*,*,#9593,.T.);
#13425=ORIENTED_EDGE('',*,*,#9599,.T.);
#13426=ORIENTED_EDGE('',*,*,#9600,.F.);
#13427=ORIENTED_EDGE('',*,*,#9601,.F.);
#13428=ORIENTED_EDGE('',*,*,#9597,.T.);
#13429=ORIENTED_EDGE('',*,*,#9602,.T.);
#13430=ORIENTED_EDGE('',*,*,#9595,.F.);
#13431=ORIENTED_EDGE('',*,*,#9603,.F.);
#13432=ORIENTED_EDGE('',*,*,#9600,.T.);
#13433=ORIENTED_EDGE('',*,*,#9594,.T.);
#13434=ORIENTED_EDGE('',*,*,#9598,.T.);
#13435=ORIENTED_EDGE('',*,*,#9601,.T.);
#13436=ORIENTED_EDGE('',*,*,#9603,.T.);
#13437=ORIENTED_EDGE('',*,*,#9592,.F.);
#13438=ORIENTED_EDGE('',*,*,#9602,.F.);
#13439=ORIENTED_EDGE('',*,*,#9599,.F.);
#13440=ORIENTED_EDGE('',*,*,#9596,.F.);
#13441=ORIENTED_EDGE('',*,*,#9604,.T.);
#13442=ORIENTED_EDGE('',*,*,#9605,.F.);
#13443=ORIENTED_EDGE('',*,*,#9606,.F.);
#13444=ORIENTED_EDGE('',*,*,#9607,.T.);
#13445=ORIENTED_EDGE('',*,*,#9608,.T.);
#13446=ORIENTED_EDGE('',*,*,#9609,.F.);
#13447=ORIENTED_EDGE('',*,*,#9610,.F.);
#13448=ORIENTED_EDGE('',*,*,#9605,.T.);
#13449=ORIENTED_EDGE('',*,*,#9611,.T.);
#13450=ORIENTED_EDGE('',*,*,#9612,.F.);
#13451=ORIENTED_EDGE('',*,*,#9613,.F.);
#13452=ORIENTED_EDGE('',*,*,#9609,.T.);
#13453=ORIENTED_EDGE('',*,*,#9614,.T.);
#13454=ORIENTED_EDGE('',*,*,#9607,.F.);
#13455=ORIENTED_EDGE('',*,*,#9615,.F.);
#13456=ORIENTED_EDGE('',*,*,#9612,.T.);
#13457=ORIENTED_EDGE('',*,*,#9606,.T.);
#13458=ORIENTED_EDGE('',*,*,#9610,.T.);
#13459=ORIENTED_EDGE('',*,*,#9613,.T.);
#13460=ORIENTED_EDGE('',*,*,#9615,.T.);
#13461=ORIENTED_EDGE('',*,*,#9604,.F.);
#13462=ORIENTED_EDGE('',*,*,#9614,.F.);
#13463=ORIENTED_EDGE('',*,*,#9611,.F.);
#13464=ORIENTED_EDGE('',*,*,#9608,.F.);
#13465=ORIENTED_EDGE('',*,*,#9616,.T.);
#13466=ORIENTED_EDGE('',*,*,#9617,.F.);
#13467=ORIENTED_EDGE('',*,*,#9618,.F.);
#13468=ORIENTED_EDGE('',*,*,#9619,.T.);
#13469=ORIENTED_EDGE('',*,*,#9620,.T.);
#13470=ORIENTED_EDGE('',*,*,#9621,.F.);
#13471=ORIENTED_EDGE('',*,*,#9622,.F.);
#13472=ORIENTED_EDGE('',*,*,#9617,.T.);
#13473=ORIENTED_EDGE('',*,*,#9623,.T.);
#13474=ORIENTED_EDGE('',*,*,#9624,.F.);
#13475=ORIENTED_EDGE('',*,*,#9625,.F.);
#13476=ORIENTED_EDGE('',*,*,#9621,.T.);
#13477=ORIENTED_EDGE('',*,*,#9626,.T.);
#13478=ORIENTED_EDGE('',*,*,#9619,.F.);
#13479=ORIENTED_EDGE('',*,*,#9627,.F.);
#13480=ORIENTED_EDGE('',*,*,#9624,.T.);
#13481=ORIENTED_EDGE('',*,*,#9618,.T.);
#13482=ORIENTED_EDGE('',*,*,#9622,.T.);
#13483=ORIENTED_EDGE('',*,*,#9625,.T.);
#13484=ORIENTED_EDGE('',*,*,#9627,.T.);
#13485=ORIENTED_EDGE('',*,*,#9616,.F.);
#13486=ORIENTED_EDGE('',*,*,#9626,.F.);
#13487=ORIENTED_EDGE('',*,*,#9623,.F.);
#13488=ORIENTED_EDGE('',*,*,#9620,.F.);
#13489=ORIENTED_EDGE('',*,*,#9628,.T.);
#13490=ORIENTED_EDGE('',*,*,#9629,.F.);
#13491=ORIENTED_EDGE('',*,*,#9630,.F.);
#13492=ORIENTED_EDGE('',*,*,#9631,.T.);
#13493=ORIENTED_EDGE('',*,*,#9632,.T.);
#13494=ORIENTED_EDGE('',*,*,#9633,.F.);
#13495=ORIENTED_EDGE('',*,*,#9634,.F.);
#13496=ORIENTED_EDGE('',*,*,#9629,.T.);
#13497=ORIENTED_EDGE('',*,*,#9635,.T.);
#13498=ORIENTED_EDGE('',*,*,#9636,.F.);
#13499=ORIENTED_EDGE('',*,*,#9637,.F.);
#13500=ORIENTED_EDGE('',*,*,#9633,.T.);
#13501=ORIENTED_EDGE('',*,*,#9638,.T.);
#13502=ORIENTED_EDGE('',*,*,#9631,.F.);
#13503=ORIENTED_EDGE('',*,*,#9639,.F.);
#13504=ORIENTED_EDGE('',*,*,#9636,.T.);
#13505=ORIENTED_EDGE('',*,*,#9630,.T.);
#13506=ORIENTED_EDGE('',*,*,#9634,.T.);
#13507=ORIENTED_EDGE('',*,*,#9637,.T.);
#13508=ORIENTED_EDGE('',*,*,#9639,.T.);
#13509=ORIENTED_EDGE('',*,*,#9628,.F.);
#13510=ORIENTED_EDGE('',*,*,#9638,.F.);
#13511=ORIENTED_EDGE('',*,*,#9635,.F.);
#13512=ORIENTED_EDGE('',*,*,#9632,.F.);
#13513=ORIENTED_EDGE('',*,*,#9640,.T.);
#13514=ORIENTED_EDGE('',*,*,#9641,.F.);
#13515=ORIENTED_EDGE('',*,*,#9642,.F.);
#13516=ORIENTED_EDGE('',*,*,#9643,.T.);
#13517=ORIENTED_EDGE('',*,*,#9644,.T.);
#13518=ORIENTED_EDGE('',*,*,#9645,.F.);
#13519=ORIENTED_EDGE('',*,*,#9646,.F.);
#13520=ORIENTED_EDGE('',*,*,#9641,.T.);
#13521=ORIENTED_EDGE('',*,*,#9647,.T.);
#13522=ORIENTED_EDGE('',*,*,#9648,.F.);
#13523=ORIENTED_EDGE('',*,*,#9649,.F.);
#13524=ORIENTED_EDGE('',*,*,#9645,.T.);
#13525=ORIENTED_EDGE('',*,*,#9650,.T.);
#13526=ORIENTED_EDGE('',*,*,#9643,.F.);
#13527=ORIENTED_EDGE('',*,*,#9651,.F.);
#13528=ORIENTED_EDGE('',*,*,#9648,.T.);
#13529=ORIENTED_EDGE('',*,*,#9642,.T.);
#13530=ORIENTED_EDGE('',*,*,#9646,.T.);
#13531=ORIENTED_EDGE('',*,*,#9649,.T.);
#13532=ORIENTED_EDGE('',*,*,#9651,.T.);
#13533=ORIENTED_EDGE('',*,*,#9640,.F.);
#13534=ORIENTED_EDGE('',*,*,#9650,.F.);
#13535=ORIENTED_EDGE('',*,*,#9647,.F.);
#13536=ORIENTED_EDGE('',*,*,#9644,.F.);
#13537=ORIENTED_EDGE('',*,*,#9652,.T.);
#13538=ORIENTED_EDGE('',*,*,#9653,.F.);
#13539=ORIENTED_EDGE('',*,*,#9654,.F.);
#13540=ORIENTED_EDGE('',*,*,#9655,.T.);
#13541=ORIENTED_EDGE('',*,*,#9656,.T.);
#13542=ORIENTED_EDGE('',*,*,#9657,.F.);
#13543=ORIENTED_EDGE('',*,*,#9658,.F.);
#13544=ORIENTED_EDGE('',*,*,#9653,.T.);
#13545=ORIENTED_EDGE('',*,*,#9659,.T.);
#13546=ORIENTED_EDGE('',*,*,#9660,.F.);
#13547=ORIENTED_EDGE('',*,*,#9661,.F.);
#13548=ORIENTED_EDGE('',*,*,#9657,.T.);
#13549=ORIENTED_EDGE('',*,*,#9662,.T.);
#13550=ORIENTED_EDGE('',*,*,#9655,.F.);
#13551=ORIENTED_EDGE('',*,*,#9663,.F.);
#13552=ORIENTED_EDGE('',*,*,#9660,.T.);
#13553=ORIENTED_EDGE('',*,*,#9654,.T.);
#13554=ORIENTED_EDGE('',*,*,#9658,.T.);
#13555=ORIENTED_EDGE('',*,*,#9661,.T.);
#13556=ORIENTED_EDGE('',*,*,#9663,.T.);
#13557=ORIENTED_EDGE('',*,*,#9652,.F.);
#13558=ORIENTED_EDGE('',*,*,#9662,.F.);
#13559=ORIENTED_EDGE('',*,*,#9659,.F.);
#13560=ORIENTED_EDGE('',*,*,#9656,.F.);
#13561=ORIENTED_EDGE('',*,*,#9664,.F.);
#13562=ORIENTED_EDGE('',*,*,#9665,.F.);
#13563=ORIENTED_EDGE('',*,*,#9666,.T.);
#13564=ORIENTED_EDGE('',*,*,#9667,.T.);
#13565=ORIENTED_EDGE('',*,*,#9668,.F.);
#13566=ORIENTED_EDGE('',*,*,#9667,.F.);
#13567=ORIENTED_EDGE('',*,*,#9669,.T.);
#13568=ORIENTED_EDGE('',*,*,#9670,.T.);
#13569=ORIENTED_EDGE('',*,*,#9671,.F.);
#13570=ORIENTED_EDGE('',*,*,#9670,.F.);
#13571=ORIENTED_EDGE('',*,*,#9672,.T.);
#13572=ORIENTED_EDGE('',*,*,#9673,.T.);
#13573=ORIENTED_EDGE('',*,*,#9674,.F.);
#13574=ORIENTED_EDGE('',*,*,#9673,.F.);
#13575=ORIENTED_EDGE('',*,*,#9675,.T.);
#13576=ORIENTED_EDGE('',*,*,#9665,.T.);
#13577=ORIENTED_EDGE('',*,*,#9666,.F.);
#13578=ORIENTED_EDGE('',*,*,#9675,.F.);
#13579=ORIENTED_EDGE('',*,*,#9672,.F.);
#13580=ORIENTED_EDGE('',*,*,#9669,.F.);
#13581=ORIENTED_EDGE('',*,*,#9664,.T.);
#13582=ORIENTED_EDGE('',*,*,#9668,.T.);
#13583=ORIENTED_EDGE('',*,*,#9671,.T.);
#13584=ORIENTED_EDGE('',*,*,#9674,.T.);
#13585=ORIENTED_EDGE('',*,*,#9676,.F.);
#13586=ORIENTED_EDGE('',*,*,#9677,.F.);
#13587=ORIENTED_EDGE('',*,*,#9678,.T.);
#13588=ORIENTED_EDGE('',*,*,#9679,.T.);
#13589=ORIENTED_EDGE('',*,*,#9680,.F.);
#13590=ORIENTED_EDGE('',*,*,#9679,.F.);
#13591=ORIENTED_EDGE('',*,*,#9681,.T.);
#13592=ORIENTED_EDGE('',*,*,#9682,.T.);
#13593=ORIENTED_EDGE('',*,*,#9683,.F.);
#13594=ORIENTED_EDGE('',*,*,#9682,.F.);
#13595=ORIENTED_EDGE('',*,*,#9684,.T.);
#13596=ORIENTED_EDGE('',*,*,#9685,.T.);
#13597=ORIENTED_EDGE('',*,*,#9686,.F.);
#13598=ORIENTED_EDGE('',*,*,#9685,.F.);
#13599=ORIENTED_EDGE('',*,*,#9687,.T.);
#13600=ORIENTED_EDGE('',*,*,#9677,.T.);
#13601=ORIENTED_EDGE('',*,*,#9678,.F.);
#13602=ORIENTED_EDGE('',*,*,#9687,.F.);
#13603=ORIENTED_EDGE('',*,*,#9684,.F.);
#13604=ORIENTED_EDGE('',*,*,#9681,.F.);
#13605=ORIENTED_EDGE('',*,*,#9676,.T.);
#13606=ORIENTED_EDGE('',*,*,#9680,.T.);
#13607=ORIENTED_EDGE('',*,*,#9683,.T.);
#13608=ORIENTED_EDGE('',*,*,#9686,.T.);
#13609=ORIENTED_EDGE('',*,*,#9688,.F.);
#13610=ORIENTED_EDGE('',*,*,#9689,.F.);
#13611=ORIENTED_EDGE('',*,*,#9690,.T.);
#13612=ORIENTED_EDGE('',*,*,#9691,.T.);
#13613=ORIENTED_EDGE('',*,*,#9692,.F.);
#13614=ORIENTED_EDGE('',*,*,#9691,.F.);
#13615=ORIENTED_EDGE('',*,*,#9693,.T.);
#13616=ORIENTED_EDGE('',*,*,#9694,.T.);
#13617=ORIENTED_EDGE('',*,*,#9695,.F.);
#13618=ORIENTED_EDGE('',*,*,#9694,.F.);
#13619=ORIENTED_EDGE('',*,*,#9696,.T.);
#13620=ORIENTED_EDGE('',*,*,#9697,.T.);
#13621=ORIENTED_EDGE('',*,*,#9698,.F.);
#13622=ORIENTED_EDGE('',*,*,#9697,.F.);
#13623=ORIENTED_EDGE('',*,*,#9699,.T.);
#13624=ORIENTED_EDGE('',*,*,#9689,.T.);
#13625=ORIENTED_EDGE('',*,*,#9690,.F.);
#13626=ORIENTED_EDGE('',*,*,#9699,.F.);
#13627=ORIENTED_EDGE('',*,*,#9696,.F.);
#13628=ORIENTED_EDGE('',*,*,#9693,.F.);
#13629=ORIENTED_EDGE('',*,*,#9688,.T.);
#13630=ORIENTED_EDGE('',*,*,#9692,.T.);
#13631=ORIENTED_EDGE('',*,*,#9695,.T.);
#13632=ORIENTED_EDGE('',*,*,#9698,.T.);
#13633=ORIENTED_EDGE('',*,*,#9700,.F.);
#13634=ORIENTED_EDGE('',*,*,#9701,.F.);
#13635=ORIENTED_EDGE('',*,*,#9702,.T.);
#13636=ORIENTED_EDGE('',*,*,#9703,.T.);
#13637=ORIENTED_EDGE('',*,*,#9704,.F.);
#13638=ORIENTED_EDGE('',*,*,#9703,.F.);
#13639=ORIENTED_EDGE('',*,*,#9705,.T.);
#13640=ORIENTED_EDGE('',*,*,#9706,.T.);
#13641=ORIENTED_EDGE('',*,*,#9707,.F.);
#13642=ORIENTED_EDGE('',*,*,#9706,.F.);
#13643=ORIENTED_EDGE('',*,*,#9708,.T.);
#13644=ORIENTED_EDGE('',*,*,#9709,.T.);
#13645=ORIENTED_EDGE('',*,*,#9710,.F.);
#13646=ORIENTED_EDGE('',*,*,#9709,.F.);
#13647=ORIENTED_EDGE('',*,*,#9711,.T.);
#13648=ORIENTED_EDGE('',*,*,#9701,.T.);
#13649=ORIENTED_EDGE('',*,*,#9702,.F.);
#13650=ORIENTED_EDGE('',*,*,#9711,.F.);
#13651=ORIENTED_EDGE('',*,*,#9708,.F.);
#13652=ORIENTED_EDGE('',*,*,#9705,.F.);
#13653=ORIENTED_EDGE('',*,*,#9700,.T.);
#13654=ORIENTED_EDGE('',*,*,#9704,.T.);
#13655=ORIENTED_EDGE('',*,*,#9707,.T.);
#13656=ORIENTED_EDGE('',*,*,#9710,.T.);
#13657=ORIENTED_EDGE('',*,*,#9712,.F.);
#13658=ORIENTED_EDGE('',*,*,#9713,.F.);
#13659=ORIENTED_EDGE('',*,*,#9714,.T.);
#13660=ORIENTED_EDGE('',*,*,#9715,.T.);
#13661=ORIENTED_EDGE('',*,*,#9716,.F.);
#13662=ORIENTED_EDGE('',*,*,#9715,.F.);
#13663=ORIENTED_EDGE('',*,*,#9717,.T.);
#13664=ORIENTED_EDGE('',*,*,#9718,.T.);
#13665=ORIENTED_EDGE('',*,*,#9719,.F.);
#13666=ORIENTED_EDGE('',*,*,#9718,.F.);
#13667=ORIENTED_EDGE('',*,*,#9720,.T.);
#13668=ORIENTED_EDGE('',*,*,#9721,.T.);
#13669=ORIENTED_EDGE('',*,*,#9722,.F.);
#13670=ORIENTED_EDGE('',*,*,#9721,.F.);
#13671=ORIENTED_EDGE('',*,*,#9723,.T.);
#13672=ORIENTED_EDGE('',*,*,#9713,.T.);
#13673=ORIENTED_EDGE('',*,*,#9714,.F.);
#13674=ORIENTED_EDGE('',*,*,#9723,.F.);
#13675=ORIENTED_EDGE('',*,*,#9720,.F.);
#13676=ORIENTED_EDGE('',*,*,#9717,.F.);
#13677=ORIENTED_EDGE('',*,*,#9712,.T.);
#13678=ORIENTED_EDGE('',*,*,#9716,.T.);
#13679=ORIENTED_EDGE('',*,*,#9719,.T.);
#13680=ORIENTED_EDGE('',*,*,#9722,.T.);
#13681=ORIENTED_EDGE('',*,*,#9724,.T.);
#13682=ORIENTED_EDGE('',*,*,#9725,.F.);
#13683=ORIENTED_EDGE('',*,*,#9726,.F.);
#13684=ORIENTED_EDGE('',*,*,#9727,.T.);
#13685=ORIENTED_EDGE('',*,*,#9728,.T.);
#13686=ORIENTED_EDGE('',*,*,#9729,.F.);
#13687=ORIENTED_EDGE('',*,*,#9730,.F.);
#13688=ORIENTED_EDGE('',*,*,#9725,.T.);
#13689=ORIENTED_EDGE('',*,*,#9731,.T.);
#13690=ORIENTED_EDGE('',*,*,#9732,.F.);
#13691=ORIENTED_EDGE('',*,*,#9733,.F.);
#13692=ORIENTED_EDGE('',*,*,#9729,.T.);
#13693=ORIENTED_EDGE('',*,*,#9734,.T.);
#13694=ORIENTED_EDGE('',*,*,#9727,.F.);
#13695=ORIENTED_EDGE('',*,*,#9735,.F.);
#13696=ORIENTED_EDGE('',*,*,#9732,.T.);
#13697=ORIENTED_EDGE('',*,*,#9726,.T.);
#13698=ORIENTED_EDGE('',*,*,#9730,.T.);
#13699=ORIENTED_EDGE('',*,*,#9733,.T.);
#13700=ORIENTED_EDGE('',*,*,#9735,.T.);
#13701=ORIENTED_EDGE('',*,*,#9724,.F.);
#13702=ORIENTED_EDGE('',*,*,#9734,.F.);
#13703=ORIENTED_EDGE('',*,*,#9731,.F.);
#13704=ORIENTED_EDGE('',*,*,#9728,.F.);
#13705=ORIENTED_EDGE('',*,*,#9736,.T.);
#13706=ORIENTED_EDGE('',*,*,#9737,.F.);
#13707=ORIENTED_EDGE('',*,*,#9738,.F.);
#13708=ORIENTED_EDGE('',*,*,#9739,.T.);
#13709=ORIENTED_EDGE('',*,*,#9740,.T.);
#13710=ORIENTED_EDGE('',*,*,#9741,.F.);
#13711=ORIENTED_EDGE('',*,*,#9742,.F.);
#13712=ORIENTED_EDGE('',*,*,#9737,.T.);
#13713=ORIENTED_EDGE('',*,*,#9743,.T.);
#13714=ORIENTED_EDGE('',*,*,#9744,.F.);
#13715=ORIENTED_EDGE('',*,*,#9745,.F.);
#13716=ORIENTED_EDGE('',*,*,#9741,.T.);
#13717=ORIENTED_EDGE('',*,*,#9746,.T.);
#13718=ORIENTED_EDGE('',*,*,#9739,.F.);
#13719=ORIENTED_EDGE('',*,*,#9747,.F.);
#13720=ORIENTED_EDGE('',*,*,#9744,.T.);
#13721=ORIENTED_EDGE('',*,*,#9738,.T.);
#13722=ORIENTED_EDGE('',*,*,#9742,.T.);
#13723=ORIENTED_EDGE('',*,*,#9745,.T.);
#13724=ORIENTED_EDGE('',*,*,#9747,.T.);
#13725=ORIENTED_EDGE('',*,*,#9736,.F.);
#13726=ORIENTED_EDGE('',*,*,#9746,.F.);
#13727=ORIENTED_EDGE('',*,*,#9743,.F.);
#13728=ORIENTED_EDGE('',*,*,#9740,.F.);
#13729=ORIENTED_EDGE('',*,*,#9748,.T.);
#13730=ORIENTED_EDGE('',*,*,#9749,.F.);
#13731=ORIENTED_EDGE('',*,*,#9750,.F.);
#13732=ORIENTED_EDGE('',*,*,#9751,.T.);
#13733=ORIENTED_EDGE('',*,*,#9752,.T.);
#13734=ORIENTED_EDGE('',*,*,#9753,.F.);
#13735=ORIENTED_EDGE('',*,*,#9754,.F.);
#13736=ORIENTED_EDGE('',*,*,#9749,.T.);
#13737=ORIENTED_EDGE('',*,*,#9755,.T.);
#13738=ORIENTED_EDGE('',*,*,#9756,.F.);
#13739=ORIENTED_EDGE('',*,*,#9757,.F.);
#13740=ORIENTED_EDGE('',*,*,#9753,.T.);
#13741=ORIENTED_EDGE('',*,*,#9758,.T.);
#13742=ORIENTED_EDGE('',*,*,#9751,.F.);
#13743=ORIENTED_EDGE('',*,*,#9759,.F.);
#13744=ORIENTED_EDGE('',*,*,#9756,.T.);
#13745=ORIENTED_EDGE('',*,*,#9750,.T.);
#13746=ORIENTED_EDGE('',*,*,#9754,.T.);
#13747=ORIENTED_EDGE('',*,*,#9757,.T.);
#13748=ORIENTED_EDGE('',*,*,#9759,.T.);
#13749=ORIENTED_EDGE('',*,*,#9748,.F.);
#13750=ORIENTED_EDGE('',*,*,#9758,.F.);
#13751=ORIENTED_EDGE('',*,*,#9755,.F.);
#13752=ORIENTED_EDGE('',*,*,#9752,.F.);
#13753=ORIENTED_EDGE('',*,*,#9760,.T.);
#13754=ORIENTED_EDGE('',*,*,#9761,.F.);
#13755=ORIENTED_EDGE('',*,*,#9762,.F.);
#13756=ORIENTED_EDGE('',*,*,#9763,.T.);
#13757=ORIENTED_EDGE('',*,*,#9764,.T.);
#13758=ORIENTED_EDGE('',*,*,#9765,.F.);
#13759=ORIENTED_EDGE('',*,*,#9766,.F.);
#13760=ORIENTED_EDGE('',*,*,#9761,.T.);
#13761=ORIENTED_EDGE('',*,*,#9767,.T.);
#13762=ORIENTED_EDGE('',*,*,#9768,.F.);
#13763=ORIENTED_EDGE('',*,*,#9769,.F.);
#13764=ORIENTED_EDGE('',*,*,#9765,.T.);
#13765=ORIENTED_EDGE('',*,*,#9770,.T.);
#13766=ORIENTED_EDGE('',*,*,#9763,.F.);
#13767=ORIENTED_EDGE('',*,*,#9771,.F.);
#13768=ORIENTED_EDGE('',*,*,#9768,.T.);
#13769=ORIENTED_EDGE('',*,*,#9762,.T.);
#13770=ORIENTED_EDGE('',*,*,#9766,.T.);
#13771=ORIENTED_EDGE('',*,*,#9769,.T.);
#13772=ORIENTED_EDGE('',*,*,#9771,.T.);
#13773=ORIENTED_EDGE('',*,*,#9760,.F.);
#13774=ORIENTED_EDGE('',*,*,#9770,.F.);
#13775=ORIENTED_EDGE('',*,*,#9767,.F.);
#13776=ORIENTED_EDGE('',*,*,#9764,.F.);
#13777=ORIENTED_EDGE('',*,*,#9772,.T.);
#13778=ORIENTED_EDGE('',*,*,#9773,.F.);
#13779=ORIENTED_EDGE('',*,*,#9774,.F.);
#13780=ORIENTED_EDGE('',*,*,#9775,.T.);
#13781=ORIENTED_EDGE('',*,*,#9776,.T.);
#13782=ORIENTED_EDGE('',*,*,#9777,.F.);
#13783=ORIENTED_EDGE('',*,*,#9778,.F.);
#13784=ORIENTED_EDGE('',*,*,#9773,.T.);
#13785=ORIENTED_EDGE('',*,*,#9779,.T.);
#13786=ORIENTED_EDGE('',*,*,#9780,.F.);
#13787=ORIENTED_EDGE('',*,*,#9781,.F.);
#13788=ORIENTED_EDGE('',*,*,#9777,.T.);
#13789=ORIENTED_EDGE('',*,*,#9782,.T.);
#13790=ORIENTED_EDGE('',*,*,#9775,.F.);
#13791=ORIENTED_EDGE('',*,*,#9783,.F.);
#13792=ORIENTED_EDGE('',*,*,#9780,.T.);
#13793=ORIENTED_EDGE('',*,*,#9774,.T.);
#13794=ORIENTED_EDGE('',*,*,#9778,.T.);
#13795=ORIENTED_EDGE('',*,*,#9781,.T.);
#13796=ORIENTED_EDGE('',*,*,#9783,.T.);
#13797=ORIENTED_EDGE('',*,*,#9772,.F.);
#13798=ORIENTED_EDGE('',*,*,#9782,.F.);
#13799=ORIENTED_EDGE('',*,*,#9779,.F.);
#13800=ORIENTED_EDGE('',*,*,#9776,.F.);
#13801=ORIENTED_EDGE('',*,*,#9784,.T.);
#13802=ORIENTED_EDGE('',*,*,#9785,.F.);
#13803=ORIENTED_EDGE('',*,*,#9786,.F.);
#13804=ORIENTED_EDGE('',*,*,#9787,.T.);
#13805=ORIENTED_EDGE('',*,*,#9788,.T.);
#13806=ORIENTED_EDGE('',*,*,#9789,.F.);
#13807=ORIENTED_EDGE('',*,*,#9790,.F.);
#13808=ORIENTED_EDGE('',*,*,#9785,.T.);
#13809=ORIENTED_EDGE('',*,*,#9791,.T.);
#13810=ORIENTED_EDGE('',*,*,#9792,.F.);
#13811=ORIENTED_EDGE('',*,*,#9793,.F.);
#13812=ORIENTED_EDGE('',*,*,#9789,.T.);
#13813=ORIENTED_EDGE('',*,*,#9794,.T.);
#13814=ORIENTED_EDGE('',*,*,#9787,.F.);
#13815=ORIENTED_EDGE('',*,*,#9795,.F.);
#13816=ORIENTED_EDGE('',*,*,#9792,.T.);
#13817=ORIENTED_EDGE('',*,*,#9786,.T.);
#13818=ORIENTED_EDGE('',*,*,#9790,.T.);
#13819=ORIENTED_EDGE('',*,*,#9793,.T.);
#13820=ORIENTED_EDGE('',*,*,#9795,.T.);
#13821=ORIENTED_EDGE('',*,*,#9784,.F.);
#13822=ORIENTED_EDGE('',*,*,#9794,.F.);
#13823=ORIENTED_EDGE('',*,*,#9791,.F.);
#13824=ORIENTED_EDGE('',*,*,#9788,.F.);
#13825=ORIENTED_EDGE('',*,*,#9796,.F.);
#13826=ORIENTED_EDGE('',*,*,#9797,.F.);
#13827=ORIENTED_EDGE('',*,*,#9798,.T.);
#13828=ORIENTED_EDGE('',*,*,#9799,.F.);
#13829=ORIENTED_EDGE('',*,*,#9798,.F.);
#13830=ORIENTED_EDGE('',*,*,#9800,.F.);
#13831=ORIENTED_EDGE('',*,*,#9801,.F.);
#13832=ORIENTED_EDGE('',*,*,#9802,.F.);
#13833=ORIENTED_EDGE('',*,*,#9803,.T.);
#13834=ORIENTED_EDGE('',*,*,#9804,.F.);
#13835=ORIENTED_EDGE('',*,*,#9803,.F.);
#13836=ORIENTED_EDGE('',*,*,#9805,.F.);
#13837=ORIENTED_EDGE('',*,*,#9806,.F.);
#13838=ORIENTED_EDGE('',*,*,#9807,.F.);
#13839=ORIENTED_EDGE('',*,*,#9808,.F.);
#13840=ORIENTED_EDGE('',*,*,#9809,.T.);
#13841=ORIENTED_EDGE('',*,*,#9810,.T.);
#13842=ORIENTED_EDGE('',*,*,#9809,.F.);
#13843=ORIENTED_EDGE('',*,*,#9796,.T.);
#13844=ORIENTED_EDGE('',*,*,#9797,.T.);
#13845=ORIENTED_EDGE('',*,*,#9811,.T.);
#13846=ORIENTED_EDGE('',*,*,#9808,.T.);
#13847=ORIENTED_EDGE('',*,*,#9811,.F.);
#13848=ORIENTED_EDGE('',*,*,#9804,.T.);
#13849=ORIENTED_EDGE('',*,*,#9799,.T.);
#13850=ORIENTED_EDGE('',*,*,#9810,.F.);
#13851=ORIENTED_EDGE('',*,*,#9812,.T.);
#13852=ORIENTED_EDGE('',*,*,#9805,.T.);
#13853=ORIENTED_EDGE('',*,*,#9813,.T.);
#13854=ORIENTED_EDGE('',*,*,#9814,.T.);
#13855=ORIENTED_EDGE('',*,*,#9815,.T.);
#13856=ORIENTED_EDGE('',*,*,#9806,.T.);
#13857=ORIENTED_EDGE('',*,*,#9816,.T.);
#13858=ORIENTED_EDGE('',*,*,#9817,.T.);
#13859=ORIENTED_EDGE('',*,*,#9807,.T.);
#13860=ORIENTED_EDGE('',*,*,#9818,.T.);
#13861=ORIENTED_EDGE('',*,*,#9819,.T.);
#13862=ORIENTED_EDGE('',*,*,#9800,.T.);
#13863=ORIENTED_EDGE('',*,*,#9820,.T.);
#13864=ORIENTED_EDGE('',*,*,#9821,.T.);
#13865=ORIENTED_EDGE('',*,*,#9801,.T.);
#13866=ORIENTED_EDGE('',*,*,#9822,.T.);
#13867=ORIENTED_EDGE('',*,*,#9823,.T.);
#13868=ORIENTED_EDGE('',*,*,#9802,.T.);
#13869=ORIENTED_EDGE('',*,*,#9824,.F.);
#13870=ORIENTED_EDGE('',*,*,#9825,.F.);
#13871=ORIENTED_EDGE('',*,*,#9826,.F.);
#13872=ORIENTED_EDGE('',*,*,#9827,.F.);
#13873=ORIENTED_EDGE('',*,*,#9828,.T.);
#13874=ORIENTED_EDGE('',*,*,#9829,.F.);
#13875=ORIENTED_EDGE('',*,*,#9830,.T.);
#13876=ORIENTED_EDGE('',*,*,#9831,.T.);
#13877=ORIENTED_EDGE('',*,*,#9829,.T.);
#13878=ORIENTED_EDGE('',*,*,#9832,.T.);
#13879=ORIENTED_EDGE('',*,*,#9833,.T.);
#13880=ORIENTED_EDGE('',*,*,#9828,.F.);
#13881=ORIENTED_EDGE('',*,*,#9834,.T.);
#13882=ORIENTED_EDGE('',*,*,#9827,.T.);
#13883=ORIENTED_EDGE('',*,*,#9835,.T.);
#13884=ORIENTED_EDGE('',*,*,#9836,.T.);
#13885=ORIENTED_EDGE('',*,*,#9826,.T.);
#13886=ORIENTED_EDGE('',*,*,#9837,.T.);
#13887=ORIENTED_EDGE('',*,*,#9838,.T.);
#13888=ORIENTED_EDGE('',*,*,#9839,.T.);
#13889=ORIENTED_EDGE('',*,*,#9824,.T.);
#13890=ORIENTED_EDGE('',*,*,#9840,.T.);
#13891=ORIENTED_EDGE('',*,*,#9825,.T.);
#13892=ORIENTED_EDGE('',*,*,#9841,.T.);
#13893=ORIENTED_EDGE('',*,*,#9823,.F.);
#13894=ORIENTED_EDGE('',*,*,#9842,.T.);
#13895=ORIENTED_EDGE('',*,*,#9841,.F.);
#13896=ORIENTED_EDGE('',*,*,#9839,.F.);
#13897=ORIENTED_EDGE('',*,*,#9843,.F.);
#13898=ORIENTED_EDGE('',*,*,#9813,.F.);
#13899=ORIENTED_EDGE('',*,*,#9821,.F.);
#13900=ORIENTED_EDGE('',*,*,#9844,.T.);
#13901=ORIENTED_EDGE('',*,*,#9837,.F.);
#13902=ORIENTED_EDGE('',*,*,#9840,.F.);
#13903=ORIENTED_EDGE('',*,*,#9842,.F.);
#13904=ORIENTED_EDGE('',*,*,#9822,.F.);
#13905=ORIENTED_EDGE('',*,*,#9819,.F.);
#13906=ORIENTED_EDGE('',*,*,#9845,.T.);
#13907=ORIENTED_EDGE('',*,*,#9835,.F.);
#13908=ORIENTED_EDGE('',*,*,#9836,.F.);
#13909=ORIENTED_EDGE('',*,*,#9844,.F.);
#13910=ORIENTED_EDGE('',*,*,#9820,.F.);
#13911=ORIENTED_EDGE('',*,*,#9817,.F.);
#13912=ORIENTED_EDGE('',*,*,#9846,.T.);
#13913=ORIENTED_EDGE('',*,*,#9832,.F.);
#13914=ORIENTED_EDGE('',*,*,#9834,.F.);
#13915=ORIENTED_EDGE('',*,*,#9845,.F.);
#13916=ORIENTED_EDGE('',*,*,#9818,.F.);
#13917=ORIENTED_EDGE('',*,*,#9815,.F.);
#13918=ORIENTED_EDGE('',*,*,#9847,.T.);
#13919=ORIENTED_EDGE('',*,*,#9830,.F.);
#13920=ORIENTED_EDGE('',*,*,#9833,.F.);
#13921=ORIENTED_EDGE('',*,*,#9846,.F.);
#13922=ORIENTED_EDGE('',*,*,#9816,.F.);
#13923=ORIENTED_EDGE('',*,*,#9812,.F.);
#13924=ORIENTED_EDGE('',*,*,#9843,.T.);
#13925=ORIENTED_EDGE('',*,*,#9838,.F.);
#13926=ORIENTED_EDGE('',*,*,#9831,.F.);
#13927=ORIENTED_EDGE('',*,*,#9847,.F.);
#13928=ORIENTED_EDGE('',*,*,#9814,.F.);
#13929=ORIENTED_EDGE('',*,*,#9848,.F.);
#13930=ORIENTED_EDGE('',*,*,#9849,.T.);
#13931=ORIENTED_EDGE('',*,*,#9850,.T.);
#13932=ORIENTED_EDGE('',*,*,#9849,.F.);
#13933=ORIENTED_EDGE('',*,*,#9851,.F.);
#13934=ORIENTED_EDGE('',*,*,#9852,.T.);
#13935=ORIENTED_EDGE('',*,*,#9853,.T.);
#13936=ORIENTED_EDGE('',*,*,#9852,.F.);
#13937=ORIENTED_EDGE('',*,*,#9850,.F.);
#13938=ORIENTED_EDGE('',*,*,#9851,.T.);
#13939=ORIENTED_EDGE('',*,*,#9848,.T.);
#13940=ORIENTED_EDGE('',*,*,#9853,.F.);
#13941=ORIENTED_EDGE('',*,*,#9854,.F.);
#13942=ORIENTED_EDGE('',*,*,#9855,.T.);
#13943=ORIENTED_EDGE('',*,*,#9856,.T.);
#13944=ORIENTED_EDGE('',*,*,#9857,.T.);
#13945=ORIENTED_EDGE('',*,*,#9855,.F.);
#13946=ORIENTED_EDGE('',*,*,#9858,.T.);
#13947=ORIENTED_EDGE('',*,*,#9859,.T.);
#13948=ORIENTED_EDGE('',*,*,#9856,.F.);
#13949=ORIENTED_EDGE('',*,*,#9857,.F.);
#13950=ORIENTED_EDGE('',*,*,#9859,.F.);
#13951=ORIENTED_EDGE('',*,*,#9860,.T.);
#13952=ORIENTED_EDGE('',*,*,#9861,.T.);
#13953=ORIENTED_EDGE('',*,*,#9862,.T.);
#13954=ORIENTED_EDGE('',*,*,#9863,.T.);
#13955=ORIENTED_EDGE('',*,*,#9862,.F.);
#13956=ORIENTED_EDGE('',*,*,#9858,.F.);
#13957=ORIENTED_EDGE('',*,*,#9864,.T.);
#13958=ORIENTED_EDGE('',*,*,#9861,.F.);
#13959=ORIENTED_EDGE('',*,*,#9864,.F.);
#13960=ORIENTED_EDGE('',*,*,#9860,.F.);
#13961=ORIENTED_EDGE('',*,*,#9865,.T.);
#13962=ORIENTED_EDGE('',*,*,#9866,.T.);
#13963=ORIENTED_EDGE('',*,*,#9867,.T.);
#13964=ORIENTED_EDGE('',*,*,#9868,.F.);
#13965=ORIENTED_EDGE('',*,*,#9869,.F.);
#13966=ORIENTED_EDGE('',*,*,#9870,.F.);
#13967=ORIENTED_EDGE('',*,*,#9868,.T.);
#13968=ORIENTED_EDGE('',*,*,#9871,.T.);
#13969=ORIENTED_EDGE('',*,*,#9872,.T.);
#13970=ORIENTED_EDGE('',*,*,#9873,.F.);
#13971=ORIENTED_EDGE('',*,*,#9874,.F.);
#13972=ORIENTED_EDGE('',*,*,#9875,.F.);
#13973=ORIENTED_EDGE('',*,*,#9876,.F.);
#13974=ORIENTED_EDGE('',*,*,#9877,.F.);
#13975=ORIENTED_EDGE('',*,*,#9878,.T.);
#13976=ORIENTED_EDGE('',*,*,#9879,.T.);
#13977=ORIENTED_EDGE('',*,*,#9873,.T.);
#13978=ORIENTED_EDGE('',*,*,#9880,.F.);
#13979=ORIENTED_EDGE('',*,*,#9877,.T.);
#13980=ORIENTED_EDGE('',*,*,#9881,.T.);
#13981=ORIENTED_EDGE('',*,*,#9882,.T.);
#13982=ORIENTED_EDGE('',*,*,#9883,.F.);
#13983=ORIENTED_EDGE('',*,*,#9884,.F.);
#13984=ORIENTED_EDGE('',*,*,#9885,.F.);
#13985=ORIENTED_EDGE('',*,*,#9883,.T.);
#13986=ORIENTED_EDGE('',*,*,#9886,.T.);
#13987=ORIENTED_EDGE('',*,*,#9887,.T.);
#13988=ORIENTED_EDGE('',*,*,#9888,.F.);
#13989=ORIENTED_EDGE('',*,*,#9889,.F.);
#13990=ORIENTED_EDGE('',*,*,#9890,.F.);
#13991=ORIENTED_EDGE('',*,*,#9888,.T.);
#13992=ORIENTED_EDGE('',*,*,#9891,.T.);
#13993=ORIENTED_EDGE('',*,*,#9892,.T.);
#13994=ORIENTED_EDGE('',*,*,#9865,.F.);
#13995=ORIENTED_EDGE('',*,*,#9893,.F.);
#13996=ORIENTED_EDGE('',*,*,#9894,.F.);
#13997=ORIENTED_EDGE('',*,*,#9895,.F.);
#13998=ORIENTED_EDGE('',*,*,#9896,.F.);
#13999=ORIENTED_EDGE('',*,*,#9897,.F.);
#14000=ORIENTED_EDGE('',*,*,#9898,.F.);
#14001=ORIENTED_EDGE('',*,*,#9899,.T.);
#14002=ORIENTED_EDGE('',*,*,#9900,.F.);
#14003=ORIENTED_EDGE('',*,*,#9863,.F.);
#14004=ORIENTED_EDGE('',*,*,#9901,.F.);
#14005=ORIENTED_EDGE('',*,*,#9902,.F.);
#14006=ORIENTED_EDGE('',*,*,#9903,.F.);
#14007=ORIENTED_EDGE('',*,*,#9904,.F.);
#14008=ORIENTED_EDGE('',*,*,#9905,.F.);
#14009=ORIENTED_EDGE('',*,*,#9906,.F.);
#14010=ORIENTED_EDGE('',*,*,#9854,.T.);
#14011=ORIENTED_EDGE('',*,*,#9870,.T.);
#14012=ORIENTED_EDGE('',*,*,#9902,.T.);
#14013=ORIENTED_EDGE('',*,*,#9893,.T.);
#14014=ORIENTED_EDGE('',*,*,#9869,.T.);
#14015=ORIENTED_EDGE('',*,*,#9875,.T.);
#14016=ORIENTED_EDGE('',*,*,#9903,.T.);
#14017=ORIENTED_EDGE('',*,*,#9874,.T.);
#14018=ORIENTED_EDGE('',*,*,#9879,.F.);
#14019=ORIENTED_EDGE('',*,*,#9904,.T.);
#14020=ORIENTED_EDGE('',*,*,#9885,.T.);
#14021=ORIENTED_EDGE('',*,*,#9905,.T.);
#14022=ORIENTED_EDGE('',*,*,#9878,.F.);
#14023=ORIENTED_EDGE('',*,*,#9884,.T.);
#14024=ORIENTED_EDGE('',*,*,#9890,.T.);
#14025=ORIENTED_EDGE('',*,*,#9906,.T.);
#14026=ORIENTED_EDGE('',*,*,#9889,.T.);
#14027=ORIENTED_EDGE('',*,*,#9894,.T.);
#14028=ORIENTED_EDGE('',*,*,#9901,.T.);
#14029=ORIENTED_EDGE('',*,*,#9896,.T.);
#14030=ORIENTED_EDGE('',*,*,#9891,.F.);
#14031=ORIENTED_EDGE('',*,*,#9887,.F.);
#14032=ORIENTED_EDGE('',*,*,#9897,.T.);
#14033=ORIENTED_EDGE('',*,*,#9886,.F.);
#14034=ORIENTED_EDGE('',*,*,#9882,.F.);
#14035=ORIENTED_EDGE('',*,*,#9876,.T.);
#14036=ORIENTED_EDGE('',*,*,#9898,.T.);
#14037=ORIENTED_EDGE('',*,*,#9881,.F.);
#14038=ORIENTED_EDGE('',*,*,#9899,.F.);
#14039=ORIENTED_EDGE('',*,*,#9880,.T.);
#14040=ORIENTED_EDGE('',*,*,#9872,.F.);
#14041=ORIENTED_EDGE('',*,*,#9900,.T.);
#14042=ORIENTED_EDGE('',*,*,#9871,.F.);
#14043=ORIENTED_EDGE('',*,*,#9867,.F.);
#14044=ORIENTED_EDGE('',*,*,#9892,.F.);
#14045=ORIENTED_EDGE('',*,*,#9895,.T.);
#14046=ORIENTED_EDGE('',*,*,#9866,.F.);
#14047=PLANE('',#15785);
#14048=PLANE('',#15786);
#14049=PLANE('',#15787);
#14050=PLANE('',#15788);
#14051=PLANE('',#15789);
#14052=PLANE('',#15790);
#14053=PLANE('',#15791);
#14054=PLANE('',#15792);
#14055=PLANE('',#15793);
#14056=PLANE('',#15794);
#14057=PLANE('',#15795);
#14058=PLANE('',#15796);
#14059=PLANE('',#15800);
#14060=PLANE('',#15801);
#14061=PLANE('',#15802);
#14062=PLANE('',#15803);
#14063=PLANE('',#15804);
#14064=PLANE('',#15805);
#14065=PLANE('',#15806);
#14066=PLANE('',#15810);
#14067=PLANE('',#15811);
#14068=PLANE('',#15812);
#14069=PLANE('',#15813);
#14070=PLANE('',#15814);
#14071=PLANE('',#15833);
#14072=PLANE('',#15834);
#14073=PLANE('',#15835);
#14074=PLANE('',#15836);
#14075=PLANE('',#15837);
#14076=PLANE('',#15838);
#14077=PLANE('',#15854);
#14078=PLANE('',#15855);
#14079=PLANE('',#15856);
#14080=PLANE('',#15857);
#14081=PLANE('',#15858);
#14082=PLANE('',#15859);
#14083=PLANE('',#15875);
#14084=PLANE('',#15876);
#14085=PLANE('',#15877);
#14086=PLANE('',#15878);
#14087=PLANE('',#15879);
#14088=PLANE('',#15880);
#14089=PLANE('',#15881);
#14090=PLANE('',#15882);
#14091=PLANE('',#15883);
#14092=PLANE('',#15884);
#14093=PLANE('',#15885);
#14094=PLANE('',#15886);
#14095=PLANE('',#15887);
#14096=PLANE('',#15888);
#14097=PLANE('',#15889);
#14098=PLANE('',#15890);
#14099=PLANE('',#15891);
#14100=PLANE('',#15892);
#14101=PLANE('',#15893);
#14102=PLANE('',#15894);
#14103=PLANE('',#15895);
#14104=PLANE('',#15896);
#14105=PLANE('',#15897);
#14106=PLANE('',#15898);
#14107=PLANE('',#15954);
#14108=PLANE('',#15955);
#14109=PLANE('',#15956);
#14110=PLANE('',#15957);
#14111=PLANE('',#15958);
#14112=PLANE('',#15959);
#14113=PLANE('',#15966);
#14114=PLANE('',#15967);
#14115=PLANE('',#15974);
#14116=PLANE('',#15975);
#14117=PLANE('',#16018);
#14118=PLANE('',#16019);
#14119=PLANE('',#16038);
#14120=PLANE('',#16039);
#14121=PLANE('',#16042);
#14122=PLANE('',#16046);
#14123=PLANE('',#16050);
#14124=PLANE('',#16051);
#14125=PLANE('',#16052);
#14126=PLANE('',#16054);
#14127=PLANE('',#16056);
#14128=PLANE('',#16058);
#14129=PLANE('',#16059);
#14130=PLANE('',#16063);
#14131=PLANE('',#16067);
#14132=PLANE('',#16068);
#14133=PLANE('',#16069);
#14134=PLANE('',#16071);
#14135=PLANE('',#16073);
#14136=PLANE('',#16075);
#14137=PLANE('',#16076);
#14138=PLANE('',#16080);
#14139=PLANE('',#16084);
#14140=PLANE('',#16085);
#14141=PLANE('',#16086);
#14142=PLANE('',#16088);
#14143=PLANE('',#16090);
#14144=PLANE('',#16092);
#14145=PLANE('',#16102);
#14146=PLANE('',#16103);
#14147=PLANE('',#16104);
#14148=PLANE('',#16105);
#14149=PLANE('',#16106);
#14150=PLANE('',#16107);
#14151=PLANE('',#16111);
#14152=PLANE('',#16113);
#14153=PLANE('',#16115);
#14154=PLANE('',#16116);
#14155=PLANE('',#16117);
#14156=PLANE('',#16119);
#14157=PLANE('',#16120);
#14158=PLANE('',#16130);
#14159=PLANE('',#16131);
#14160=PLANE('',#16132);
#14161=PLANE('',#16133);
#14162=PLANE('',#16134);
#14163=PLANE('',#16135);
#14164=PLANE('',#16139);
#14165=PLANE('',#16141);
#14166=PLANE('',#16143);
#14167=PLANE('',#16144);
#14168=PLANE('',#16145);
#14169=PLANE('',#16147);
#14170=PLANE('',#16148);
#14171=PLANE('',#16161);
#14172=PLANE('',#16162);
#14173=PLANE('',#16163);
#14174=PLANE('',#16167);
#14175=PLANE('',#16170);
#14176=PLANE('',#16171);
#14177=PLANE('',#16172);
#14178=PLANE('',#16174);
#14179=PLANE('',#16176);
#14180=PLANE('',#16179);
#14181=PLANE('',#16180);
#14182=PLANE('',#16181);
#14183=PLANE('',#16182);
#14184=PLANE('',#16183);
#14185=PLANE('',#16187);
#14186=PLANE('',#16189);
#14187=PLANE('',#16191);
#14188=PLANE('',#16192);
#14189=PLANE('',#16193);
#14190=PLANE('',#16195);
#14191=PLANE('',#16196);
#14192=PLANE('',#16200);
#14193=PLANE('',#16202);
#14194=PLANE('',#16204);
#14195=PLANE('',#16205);
#14196=PLANE('',#16206);
#14197=PLANE('',#16208);
#14198=PLANE('',#16209);
#14199=PLANE('',#16211);
#14200=PLANE('',#16212);
#14201=PLANE('',#16216);
#14202=PLANE('',#16217);
#14203=PLANE('',#16218);
#14204=PLANE('',#16222);
#14205=PLANE('',#16223);
#14206=PLANE('',#16224);
#14207=PLANE('',#16225);
#14208=PLANE('',#16226);
#14209=PLANE('',#16227);
#14210=PLANE('',#16228);
#14211=PLANE('',#16238);
#14212=PLANE('',#16239);
#14213=PLANE('',#16240);
#14214=PLANE('',#16241);
#14215=PLANE('',#16242);
#14216=PLANE('',#16243);
#14217=PLANE('',#16253);
#14218=PLANE('',#16254);
#14219=PLANE('',#16255);
#14220=PLANE('',#16256);
#14221=PLANE('',#16257);
#14222=PLANE('',#16258);
#14223=PLANE('',#16274);
#14224=PLANE('',#16275);
#14225=PLANE('',#16282);
#14226=PLANE('',#16283);
#14227=PLANE('',#16284);
#14228=PLANE('',#16285);
#14229=PLANE('',#16286);
#14230=PLANE('',#16287);
#14231=PLANE('',#16288);
#14232=PLANE('',#16289);
#14233=PLANE('',#16302);
#14234=PLANE('',#16309);
#14235=PLANE('',#16310);
#14236=PLANE('',#16311);
#14237=PLANE('',#16312);
#14238=PLANE('',#16313);
#14239=PLANE('',#16314);
#14240=PLANE('',#16315);
#14241=PLANE('',#16316);
#14242=PLANE('',#16329);
#14243=PLANE('',#16342);
#14244=PLANE('',#16343);
#14245=PLANE('',#16344);
#14246=PLANE('',#16345);
#14247=PLANE('',#16346);
#14248=PLANE('',#16347);
#14249=PLANE('',#16348);
#14250=PLANE('',#16355);
#14251=PLANE('',#16438);
#14252=PLANE('',#16439);
#14253=PLANE('',#16440);
#14254=PLANE('',#16441);
#14255=PLANE('',#16482);
#14256=PLANE('',#16484);
#14257=PLANE('',#16486);
#14258=PLANE('',#16493);
#14259=PLANE('',#16500);
#14260=PLANE('',#16501);
#14261=PLANE('',#16502);
#14262=PLANE('',#16503);
#14263=PLANE('',#16518);
#14264=PLANE('',#16526);
#14265=PLANE('',#16527);
#14266=PLANE('',#16549);
#14267=PLANE('',#16550);
#14268=PLANE('',#16551);
#14269=PLANE('',#16552);
#14270=PLANE('',#16553);
#14271=PLANE('',#16554);
#14272=PLANE('',#16558);
#14273=PLANE('',#16560);
#14274=PLANE('',#16562);
#14275=PLANE('',#16563);
#14276=PLANE('',#16564);
#14277=PLANE('',#16565);
#14278=PLANE('',#16567);
#14279=PLANE('',#16571);
#14280=PLANE('',#16573);
#14281=PLANE('',#16575);
#14282=PLANE('',#16576);
#14283=PLANE('',#16577);
#14284=PLANE('',#16578);
#14285=PLANE('',#16580);
#14286=PLANE('',#16596);
#14287=PLANE('',#16597);
#14288=PLANE('',#16598);
#14289=PLANE('',#16599);
#14290=PLANE('',#16600);
#14291=PLANE('',#16601);
#14292=PLANE('',#16602);
#14293=PLANE('',#16603);
#14294=PLANE('',#16604);
#14295=PLANE('',#16605);
#14296=PLANE('',#16606);
#14297=PLANE('',#16607);
#14298=PLANE('',#16608);
#14299=PLANE('',#16609);
#14300=PLANE('',#16610);
#14301=PLANE('',#16611);
#14302=PLANE('',#16612);
#14303=PLANE('',#16613);
#14304=PLANE('',#16614);
#14305=PLANE('',#16615);
#14306=PLANE('',#16616);
#14307=PLANE('',#16617);
#14308=PLANE('',#16618);
#14309=PLANE('',#16619);
#14310=PLANE('',#16620);
#14311=PLANE('',#16621);
#14312=PLANE('',#16622);
#14313=PLANE('',#16623);
#14314=PLANE('',#16624);
#14315=PLANE('',#16625);
#14316=PLANE('',#16635);
#14317=PLANE('',#16636);
#14318=PLANE('',#16637);
#14319=PLANE('',#16638);
#14320=PLANE('',#16639);
#14321=PLANE('',#16640);
#14322=PLANE('',#16650);
#14323=PLANE('',#16651);
#14324=PLANE('',#16652);
#14325=PLANE('',#16653);
#14326=PLANE('',#16654);
#14327=PLANE('',#16655);
#14328=PLANE('',#16665);
#14329=PLANE('',#16666);
#14330=PLANE('',#16667);
#14331=PLANE('',#16668);
#14332=PLANE('',#16669);
#14333=PLANE('',#16670);
#14334=PLANE('',#16680);
#14335=PLANE('',#16681);
#14336=PLANE('',#16682);
#14337=PLANE('',#16683);
#14338=PLANE('',#16684);
#14339=PLANE('',#16685);
#14340=PLANE('',#16686);
#14341=PLANE('',#16687);
#14342=PLANE('',#16688);
#14343=PLANE('',#16689);
#14344=PLANE('',#16690);
#14345=PLANE('',#16691);
#14346=PLANE('',#16692);
#14347=PLANE('',#16693);
#14348=PLANE('',#16694);
#14349=PLANE('',#16695);
#14350=PLANE('',#16696);
#14351=PLANE('',#16697);
#14352=PLANE('',#16698);
#14353=PLANE('',#16699);
#14354=PLANE('',#16700);
#14355=PLANE('',#16701);
#14356=PLANE('',#16702);
#14357=PLANE('',#16703);
#14358=PLANE('',#16704);
#14359=PLANE('',#16705);
#14360=PLANE('',#16706);
#14361=PLANE('',#16707);
#14362=PLANE('',#16708);
#14363=PLANE('',#16709);
#14364=PLANE('',#16710);
#14365=PLANE('',#16711);
#14366=PLANE('',#16712);
#14367=PLANE('',#16713);
#14368=PLANE('',#16714);
#14369=PLANE('',#16715);
#14370=PLANE('',#16728);
#14371=PLANE('',#16729);
#14372=PLANE('',#16730);
#14373=PLANE('',#16731);
#14374=PLANE('',#16732);
#14375=PLANE('',#16733);
#14376=PLANE('',#16752);
#14377=PLANE('',#16753);
#14378=PLANE('',#16754);
#14379=PLANE('',#16755);
#14380=PLANE('',#16756);
#14381=PLANE('',#16757);
#14382=PLANE('',#16758);
#14383=PLANE('',#16759);
#14384=PLANE('',#16760);
#14385=PLANE('',#16761);
#14386=PLANE('',#16762);
#14387=PLANE('',#16763);
#14388=PLANE('',#16764);
#14389=PLANE('',#16765);
#14390=PLANE('',#16766);
#14391=PLANE('',#16767);
#14392=PLANE('',#16768);
#14393=PLANE('',#16769);
#14394=PLANE('',#16770);
#14395=PLANE('',#16771);
#14396=PLANE('',#16772);
#14397=PLANE('',#16773);
#14398=PLANE('',#16774);
#14399=PLANE('',#16775);
#14400=PLANE('',#16776);
#14401=PLANE('',#16777);
#14402=PLANE('',#16778);
#14403=PLANE('',#16779);
#14404=PLANE('',#16780);
#14405=PLANE('',#16781);
#14406=PLANE('',#16782);
#14407=PLANE('',#16783);
#14408=PLANE('',#16784);
#14409=PLANE('',#16785);
#14410=PLANE('',#16786);
#14411=PLANE('',#16787);
#14412=PLANE('',#16788);
#14413=PLANE('',#16789);
#14414=PLANE('',#16790);
#14415=PLANE('',#16791);
#14416=PLANE('',#16792);
#14417=PLANE('',#16793);
#14418=PLANE('',#16794);
#14419=PLANE('',#16795);
#14420=PLANE('',#16796);
#14421=PLANE('',#16797);
#14422=PLANE('',#16798);
#14423=PLANE('',#16799);
#14424=PLANE('',#16800);
#14425=PLANE('',#16801);
#14426=PLANE('',#16802);
#14427=PLANE('',#16803);
#14428=PLANE('',#16804);
#14429=PLANE('',#16805);
#14430=PLANE('',#16806);
#14431=PLANE('',#16807);
#14432=PLANE('',#16808);
#14433=PLANE('',#16809);
#14434=PLANE('',#16810);
#14435=PLANE('',#16811);
#14436=PLANE('',#16812);
#14437=PLANE('',#16813);
#14438=PLANE('',#16814);
#14439=PLANE('',#16815);
#14440=PLANE('',#16816);
#14441=PLANE('',#16817);
#14442=PLANE('',#16818);
#14443=PLANE('',#16819);
#14444=PLANE('',#16820);
#14445=PLANE('',#16821);
#14446=PLANE('',#16822);
#14447=PLANE('',#16823);
#14448=PLANE('',#16824);
#14449=PLANE('',#16825);
#14450=PLANE('',#16826);
#14451=PLANE('',#16827);
#14452=PLANE('',#16828);
#14453=PLANE('',#16829);
#14454=PLANE('',#16830);
#14455=PLANE('',#16831);
#14456=PLANE('',#16832);
#14457=PLANE('',#16833);
#14458=PLANE('',#16834);
#14459=PLANE('',#16835);
#14460=PLANE('',#16836);
#14461=PLANE('',#16837);
#14462=PLANE('',#16838);
#14463=PLANE('',#16839);
#14464=PLANE('',#16840);
#14465=PLANE('',#16841);
#14466=PLANE('',#16842);
#14467=PLANE('',#16843);
#14468=PLANE('',#16844);
#14469=PLANE('',#16845);
#14470=PLANE('',#16846);
#14471=PLANE('',#16847);
#14472=PLANE('',#16848);
#14473=PLANE('',#16849);
#14474=PLANE('',#16850);
#14475=PLANE('',#16851);
#14476=PLANE('',#16852);
#14477=PLANE('',#16853);
#14478=PLANE('',#16854);
#14479=PLANE('',#16855);
#14480=PLANE('',#16856);
#14481=PLANE('',#16869);
#14482=PLANE('',#16870);
#14483=PLANE('',#16871);
#14484=PLANE('',#16872);
#14485=PLANE('',#16873);
#14486=PLANE('',#16874);
#14487=PLANE('',#16875);
#14488=PLANE('',#16876);
#14489=PLANE('',#16877);
#14490=PLANE('',#16878);
#14491=PLANE('',#16879);
#14492=PLANE('',#16880);
#14493=PLANE('',#16881);
#14494=PLANE('',#16882);
#14495=PLANE('',#16883);
#14496=PLANE('',#16884);
#14497=PLANE('',#16885);
#14498=PLANE('',#16886);
#14499=PLANE('',#16887);
#14500=PLANE('',#16888);
#14501=PLANE('',#16889);
#14502=PLANE('',#16890);
#14503=PLANE('',#16891);
#14504=PLANE('',#16892);
#14505=PLANE('',#16893);
#14506=PLANE('',#16894);
#14507=PLANE('',#16895);
#14508=PLANE('',#16896);
#14509=PLANE('',#16897);
#14510=PLANE('',#16898);
#14511=PLANE('',#16899);
#14512=PLANE('',#16900);
#14513=PLANE('',#16901);
#14514=PLANE('',#16902);
#14515=PLANE('',#16903);
#14516=PLANE('',#16904);
#14517=PLANE('',#16905);
#14518=PLANE('',#16906);
#14519=PLANE('',#16907);
#14520=PLANE('',#16908);
#14521=PLANE('',#16909);
#14522=PLANE('',#16910);
#14523=PLANE('',#16911);
#14524=PLANE('',#16912);
#14525=PLANE('',#16913);
#14526=PLANE('',#16914);
#14527=PLANE('',#16915);
#14528=PLANE('',#16916);
#14529=PLANE('',#16917);
#14530=PLANE('',#16918);
#14531=PLANE('',#16919);
#14532=PLANE('',#16920);
#14533=PLANE('',#16921);
#14534=PLANE('',#16922);
#14535=PLANE('',#16923);
#14536=PLANE('',#16924);
#14537=PLANE('',#16925);
#14538=PLANE('',#16926);
#14539=PLANE('',#16927);
#14540=PLANE('',#16928);
#14541=PLANE('',#16929);
#14542=PLANE('',#16930);
#14543=PLANE('',#16931);
#14544=PLANE('',#16932);
#14545=PLANE('',#16933);
#14546=PLANE('',#16934);
#14547=PLANE('',#16935);
#14548=PLANE('',#16936);
#14549=PLANE('',#16937);
#14550=PLANE('',#16938);
#14551=PLANE('',#16939);
#14552=PLANE('',#16940);
#14553=PLANE('',#16941);
#14554=PLANE('',#16942);
#14555=PLANE('',#16943);
#14556=PLANE('',#16944);
#14557=PLANE('',#16945);
#14558=PLANE('',#16946);
#14559=PLANE('',#16947);
#14560=PLANE('',#16948);
#14561=PLANE('',#16949);
#14562=PLANE('',#16950);
#14563=PLANE('',#16951);
#14564=PLANE('',#16952);
#14565=PLANE('',#16953);
#14566=PLANE('',#16954);
#14567=PLANE('',#16955);
#14568=PLANE('',#16956);
#14569=PLANE('',#16957);
#14570=PLANE('',#16958);
#14571=PLANE('',#16959);
#14572=PLANE('',#16960);
#14573=PLANE('',#16961);
#14574=PLANE('',#16962);
#14575=PLANE('',#16963);
#14576=PLANE('',#16964);
#14577=PLANE('',#16965);
#14578=PLANE('',#16966);
#14579=PLANE('',#16967);
#14580=PLANE('',#16968);
#14581=PLANE('',#16969);
#14582=PLANE('',#16970);
#14583=PLANE('',#16971);
#14584=PLANE('',#16972);
#14585=PLANE('',#16973);
#14586=PLANE('',#16974);
#14587=PLANE('',#16975);
#14588=PLANE('',#16976);
#14589=PLANE('',#16977);
#14590=PLANE('',#16978);
#14591=PLANE('',#16979);
#14592=PLANE('',#16980);
#14593=PLANE('',#16981);
#14594=PLANE('',#16982);
#14595=PLANE('',#16983);
#14596=PLANE('',#16984);
#14597=PLANE('',#16985);
#14598=PLANE('',#16986);
#14599=PLANE('',#16987);
#14600=PLANE('',#16988);
#14601=PLANE('',#16989);
#14602=PLANE('',#16990);
#14603=PLANE('',#16991);
#14604=PLANE('',#16992);
#14605=PLANE('',#16993);
#14606=PLANE('',#16994);
#14607=PLANE('',#16995);
#14608=PLANE('',#16996);
#14609=PLANE('',#16997);
#14610=PLANE('',#16998);
#14611=PLANE('',#16999);
#14612=PLANE('',#17000);
#14613=PLANE('',#17001);
#14614=PLANE('',#17002);
#14615=PLANE('',#17003);
#14616=PLANE('',#17004);
#14617=PLANE('',#17005);
#14618=PLANE('',#17006);
#14619=PLANE('',#17025);
#14620=PLANE('',#17026);
#14621=PLANE('',#17027);
#14622=PLANE('',#17028);
#14623=PLANE('',#17029);
#14624=PLANE('',#17030);
#14625=PLANE('',#17031);
#14626=PLANE('',#17032);
#14627=PLANE('',#17033);
#14628=PLANE('',#17046);
#14629=PLANE('',#17047);
#14630=PLANE('',#17048);
#14631=PLANE('',#17049);
#14632=PLANE('',#17050);
#14633=PLANE('',#17051);
#14634=PLANE('',#17059);
#14635=PLANE('',#17060);
#14636=PLANE('',#17073);
#14637=PLANE('',#17074);
#14638=PLANE('',#17075);
#14639=PLANE('',#17076);
#14640=PLANE('',#17077);
#14641=PLANE('',#17078);
#14642=PLANE('',#17079);
#14643=PLANE('',#17086);
#14644=ADVANCED_FACE('',(#1676),#14047,.T.);
#14645=ADVANCED_FACE('',(#1677),#14048,.T.);
#14646=ADVANCED_FACE('',(#1678),#14049,.T.);
#14647=ADVANCED_FACE('',(#1679),#14050,.T.);
#14648=ADVANCED_FACE('',(#1680,#1469),#14051,.T.);
#14649=ADVANCED_FACE('',(#1681,#1470),#14052,.F.);
#14650=ADVANCED_FACE('',(#1682),#14053,.F.);
#14651=ADVANCED_FACE('',(#1683),#14054,.F.);
#14652=ADVANCED_FACE('',(#1684),#14055,.F.);
#14653=ADVANCED_FACE('',(#1685),#14056,.F.);
#14654=ADVANCED_FACE('',(#1686),#14057,.F.);
#14655=ADVANCED_FACE('',(#1687),#14058,.F.);
#14656=ADVANCED_FACE('',(#1688),#1081,.F.);
#14657=ADVANCED_FACE('',(#1689),#14059,.F.);
#14658=ADVANCED_FACE('',(#1690),#14060,.F.);
#14659=ADVANCED_FACE('',(#1691),#14061,.F.);
#14660=ADVANCED_FACE('',(#1692),#14062,.T.);
#14661=ADVANCED_FACE('',(#1693),#14063,.F.);
#14662=ADVANCED_FACE('',(#1694),#14064,.F.);
#14663=ADVANCED_FACE('',(#1695),#14065,.F.);
#14664=ADVANCED_FACE('',(#1696),#1082,.F.);
#14665=ADVANCED_FACE('',(#1697),#14066,.F.);
#14666=ADVANCED_FACE('',(#1698),#14067,.F.);
#14667=ADVANCED_FACE('',(#1699),#14068,.F.);
#14668=ADVANCED_FACE('',(#1700),#14069,.T.);
#14669=ADVANCED_FACE('',(#1701),#14070,.F.);
#14670=ADVANCED_FACE('',(#1702),#1083,.F.);
#14671=ADVANCED_FACE('',(#1703),#1084,.F.);
#14672=ADVANCED_FACE('',(#1704),#1085,.F.);
#14673=ADVANCED_FACE('',(#1705),#1086,.F.);
#14674=ADVANCED_FACE('',(#1706),#1087,.F.);
#14675=ADVANCED_FACE('',(#1707),#1088,.F.);
#14676=ADVANCED_FACE('',(#1708,#1471,#1472,#1473,#1474,#1475,#1476),#14071,
 .T.);
#14677=ADVANCED_FACE('',(#1709,#1477,#1478,#1479,#1480,#1481,#1482),#14072,
 .F.);
#14678=ADVANCED_FACE('',(#1710),#14073,.F.);
#14679=ADVANCED_FACE('',(#1711),#14074,.F.);
#14680=ADVANCED_FACE('',(#1712),#14075,.F.);
#14681=ADVANCED_FACE('',(#1713),#14076,.F.);
#14682=ADVANCED_FACE('',(#1714),#1089,.F.);
#14683=ADVANCED_FACE('',(#1715),#1090,.F.);
#14684=ADVANCED_FACE('',(#1716),#1091,.F.);
#14685=ADVANCED_FACE('',(#1717),#1092,.F.);
#14686=ADVANCED_FACE('',(#1718),#1093,.F.);
#14687=ADVANCED_FACE('',(#1719),#14077,.T.);
#14688=ADVANCED_FACE('',(#1720),#14078,.T.);
#14689=ADVANCED_FACE('',(#1721),#14079,.T.);
#14690=ADVANCED_FACE('',(#1722),#14080,.T.);
#14691=ADVANCED_FACE('',(#1723,#1483,#1484,#1485,#1486,#1487),#14081,.T.);
#14692=ADVANCED_FACE('',(#1724,#1488,#1489,#1490,#1491,#1492),#14082,.F.);
#14693=ADVANCED_FACE('',(#1725),#1094,.F.);
#14694=ADVANCED_FACE('',(#1726),#1095,.F.);
#14695=ADVANCED_FACE('',(#1727),#1096,.F.);
#14696=ADVANCED_FACE('',(#1728),#1097,.F.);
#14697=ADVANCED_FACE('',(#1729),#1098,.F.);
#14698=ADVANCED_FACE('',(#1730),#14083,.T.);
#14699=ADVANCED_FACE('',(#1731),#14084,.T.);
#14700=ADVANCED_FACE('',(#1732),#14085,.T.);
#14701=ADVANCED_FACE('',(#1733),#14086,.T.);
#14702=ADVANCED_FACE('',(#1734,#1493,#1494,#1495,#1496,#1497),#14087,.T.);
#14703=ADVANCED_FACE('',(#1735,#1498,#1499,#1500,#1501,#1502),#14088,.F.);
#14704=ADVANCED_FACE('',(#1736),#14089,.F.);
#14705=ADVANCED_FACE('',(#1737),#14090,.F.);
#14706=ADVANCED_FACE('',(#1738),#14091,.F.);
#14707=ADVANCED_FACE('',(#1739),#14092,.F.);
#14708=ADVANCED_FACE('',(#1740),#14093,.T.);
#14709=ADVANCED_FACE('',(#1741),#14094,.F.);
#14710=ADVANCED_FACE('',(#1742),#14095,.F.);
#14711=ADVANCED_FACE('',(#1743),#14096,.F.);
#14712=ADVANCED_FACE('',(#1744),#14097,.F.);
#14713=ADVANCED_FACE('',(#1745),#14098,.F.);
#14714=ADVANCED_FACE('',(#1746),#14099,.F.);
#14715=ADVANCED_FACE('',(#1747),#14100,.T.);
#14716=ADVANCED_FACE('',(#1748),#14101,.F.);
#14717=ADVANCED_FACE('',(#1749),#14102,.F.);
#14718=ADVANCED_FACE('',(#1750),#14103,.F.);
#14719=ADVANCED_FACE('',(#1751),#14104,.F.);
#14720=ADVANCED_FACE('',(#1752),#14105,.F.);
#14721=ADVANCED_FACE('',(#1753),#14106,.T.);
#14722=ADVANCED_FACE('',(#1754),#1099,.F.);
#14723=ADVANCED_FACE('',(#1755),#1100,.F.);
#14724=ADVANCED_FACE('',(#1756),#1101,.F.);
#14725=ADVANCED_FACE('',(#1757),#1102,.F.);
#14726=ADVANCED_FACE('',(#1758),#1103,.F.);
#14727=ADVANCED_FACE('',(#1759),#1104,.F.);
#14728=ADVANCED_FACE('',(#1760),#1105,.F.);
#14729=ADVANCED_FACE('',(#1761),#1106,.F.);
#14730=ADVANCED_FACE('',(#1762),#1107,.F.);
#14731=ADVANCED_FACE('',(#1763),#1108,.F.);
#14732=ADVANCED_FACE('',(#1764),#1109,.F.);
#14733=ADVANCED_FACE('',(#1765),#1110,.F.);
#14734=ADVANCED_FACE('',(#1766),#1111,.F.);
#14735=ADVANCED_FACE('',(#1767),#1112,.F.);
#14736=ADVANCED_FACE('',(#1768),#1113,.F.);
#14737=ADVANCED_FACE('',(#1769),#1114,.F.);
#14738=ADVANCED_FACE('',(#1770),#1115,.F.);
#14739=ADVANCED_FACE('',(#1771),#1116,.F.);
#14740=ADVANCED_FACE('',(#1772),#14107,.T.);
#14741=ADVANCED_FACE('',(#1773),#14108,.T.);
#14742=ADVANCED_FACE('',(#1774),#14109,.T.);
#14743=ADVANCED_FACE('',(#1775),#14110,.T.);
#14744=ADVANCED_FACE('',(#1776,#1503,#1504,#1505,#1506,#1507,#1508,#1509,
#1510,#1511,#1512,#1513,#1514,#1515,#1516,#1517,#1518,#1519,#1520),#14111,
 .T.);
#14745=ADVANCED_FACE('',(#1777,#1521,#1522,#1523,#1524,#1525,#1526,#1527,
#1528,#1529,#1530,#1531,#1532,#1533,#1534,#1535,#1536,#1537,#1538),#14112,
 .F.);
#14746=ADVANCED_FACE('',(#1778),#1117,.T.);
#14747=ADVANCED_FACE('',(#1779),#1118,.F.);
#14748=ADVANCED_FACE('',(#1780,#1539),#14113,.T.);
#14749=ADVANCED_FACE('',(#1781,#1540),#14114,.F.);
#14750=ADVANCED_FACE('',(#1782),#1119,.T.);
#14751=ADVANCED_FACE('',(#1783),#1120,.F.);
#14752=ADVANCED_FACE('',(#1784,#1541),#14115,.T.);
#14753=ADVANCED_FACE('',(#1785,#1542),#14116,.F.);
#14754=ADVANCED_FACE('',(#1786),#1121,.F.);
#14755=ADVANCED_FACE('',(#1787),#1122,.F.);
#14756=ADVANCED_FACE('',(#1788),#1123,.F.);
#14757=ADVANCED_FACE('',(#1789),#1124,.F.);
#14758=ADVANCED_FACE('',(#1790),#1125,.F.);
#14759=ADVANCED_FACE('',(#1791),#1126,.F.);
#14760=ADVANCED_FACE('',(#1792),#1127,.F.);
#14761=ADVANCED_FACE('',(#1793),#1128,.F.);
#14762=ADVANCED_FACE('',(#1794),#1129,.F.);
#14763=ADVANCED_FACE('',(#1795),#1130,.F.);
#14764=ADVANCED_FACE('',(#1796),#1131,.F.);
#14765=ADVANCED_FACE('',(#1797),#1132,.F.);
#14766=ADVANCED_FACE('',(#1798),#1133,.F.);
#14767=ADVANCED_FACE('',(#1799),#1134,.T.);
#14768=ADVANCED_FACE('',(#1800,#1543,#1544,#1545,#1546,#1547,#1548,#1549,
#1550,#1551,#1552,#1553,#1554,#1555),#14117,.F.);
#14769=ADVANCED_FACE('',(#1801,#1556,#1557,#1558,#1559,#1560,#1561,#1562,
#1563,#1564,#1565,#1566,#1567,#1568),#14118,.T.);
#14770=ADVANCED_FACE('',(#1802),#1135,.F.);
#14771=ADVANCED_FACE('',(#1803),#1136,.F.);
#14772=ADVANCED_FACE('',(#1804),#1137,.F.);
#14773=ADVANCED_FACE('',(#1805),#1138,.F.);
#14774=ADVANCED_FACE('',(#1806),#1139,.F.);
#14775=ADVANCED_FACE('',(#1807),#1140,.T.);
#14776=ADVANCED_FACE('',(#1808,#1569,#1570,#1571,#1572,#1573),#14119,.F.);
#14777=ADVANCED_FACE('',(#1809,#1574,#1575,#1576,#1577,#1578),#14120,.T.);
#14778=ADVANCED_FACE('',(#1810),#14121,.T.);
#14779=ADVANCED_FACE('',(#1811),#14122,.T.);
#14780=ADVANCED_FACE('',(#1812),#14123,.T.);
#14781=ADVANCED_FACE('',(#1813),#14124,.T.);
#14782=ADVANCED_FACE('',(#1814),#14125,.T.);
#14783=ADVANCED_FACE('',(#1815),#1141,.T.);
#14784=ADVANCED_FACE('',(#1816),#14126,.T.);
#14785=ADVANCED_FACE('',(#1817),#1142,.F.);
#14786=ADVANCED_FACE('',(#1818),#14127,.T.);
#14787=ADVANCED_FACE('',(#1819),#1143,.T.);
#14788=ADVANCED_FACE('',(#1820),#14128,.T.);
#14789=ADVANCED_FACE('',(#1821),#14129,.T.);
#14790=ADVANCED_FACE('',(#1822),#14130,.T.);
#14791=ADVANCED_FACE('',(#1823),#14131,.T.);
#14792=ADVANCED_FACE('',(#1824),#14132,.T.);
#14793=ADVANCED_FACE('',(#1825),#14133,.T.);
#14794=ADVANCED_FACE('',(#1826),#1144,.T.);
#14795=ADVANCED_FACE('',(#1827),#14134,.T.);
#14796=ADVANCED_FACE('',(#1828),#1145,.F.);
#14797=ADVANCED_FACE('',(#1829),#14135,.T.);
#14798=ADVANCED_FACE('',(#1830),#1146,.T.);
#14799=ADVANCED_FACE('',(#1831),#14136,.T.);
#14800=ADVANCED_FACE('',(#1832),#14137,.T.);
#14801=ADVANCED_FACE('',(#1833),#14138,.T.);
#14802=ADVANCED_FACE('',(#1834),#14139,.T.);
#14803=ADVANCED_FACE('',(#1835),#14140,.T.);
#14804=ADVANCED_FACE('',(#1836),#14141,.T.);
#14805=ADVANCED_FACE('',(#1837),#1147,.T.);
#14806=ADVANCED_FACE('',(#1838),#14142,.T.);
#14807=ADVANCED_FACE('',(#1839),#1148,.F.);
#14808=ADVANCED_FACE('',(#1840),#14143,.T.);
#14809=ADVANCED_FACE('',(#1841),#1149,.T.);
#14810=ADVANCED_FACE('',(#1842),#14144,.T.);
#14811=ADVANCED_FACE('',(#1843),#1150,.F.);
#14812=ADVANCED_FACE('',(#1844),#1151,.T.);
#14813=ADVANCED_FACE('',(#1845),#1152,.F.);
#14814=ADVANCED_FACE('',(#1846),#14145,.T.);
#14815=ADVANCED_FACE('',(#1847),#14146,.T.);
#14816=ADVANCED_FACE('',(#1848),#14147,.T.);
#14817=ADVANCED_FACE('',(#1849),#14148,.T.);
#14818=ADVANCED_FACE('',(#1850,#1579),#14149,.F.);
#14819=ADVANCED_FACE('',(#1851,#1580),#14150,.T.);
#14820=ADVANCED_FACE('',(#1852),#1153,.F.);
#14821=ADVANCED_FACE('',(#1853,#1581),#14151,.F.);
#14822=ADVANCED_FACE('',(#1854,#1582),#14152,.T.);
#14823=ADVANCED_FACE('',(#1855),#14153,.F.);
#14824=ADVANCED_FACE('',(#1856),#14154,.F.);
#14825=ADVANCED_FACE('',(#1857),#14155,.F.);
#14826=ADVANCED_FACE('',(#1858),#1154,.T.);
#14827=ADVANCED_FACE('',(#1859),#14156,.F.);
#14828=ADVANCED_FACE('',(#1860),#14157,.F.);
#14829=ADVANCED_FACE('',(#1861),#1155,.F.);
#14830=ADVANCED_FACE('',(#1862),#1156,.T.);
#14831=ADVANCED_FACE('',(#1863),#1157,.F.);
#14832=ADVANCED_FACE('',(#1864),#14158,.T.);
#14833=ADVANCED_FACE('',(#1865),#14159,.T.);
#14834=ADVANCED_FACE('',(#1866),#14160,.T.);
#14835=ADVANCED_FACE('',(#1867),#14161,.T.);
#14836=ADVANCED_FACE('',(#1868,#1583),#14162,.F.);
#14837=ADVANCED_FACE('',(#1869,#1584),#14163,.T.);
#14838=ADVANCED_FACE('',(#1870),#1158,.F.);
#14839=ADVANCED_FACE('',(#1871,#1585),#14164,.F.);
#14840=ADVANCED_FACE('',(#1872,#1586),#14165,.T.);
#14841=ADVANCED_FACE('',(#1873),#14166,.F.);
#14842=ADVANCED_FACE('',(#1874),#14167,.F.);
#14843=ADVANCED_FACE('',(#1875),#14168,.F.);
#14844=ADVANCED_FACE('',(#1876),#1159,.T.);
#14845=ADVANCED_FACE('',(#1877),#14169,.F.);
#14846=ADVANCED_FACE('',(#1878),#14170,.F.);
#14847=ADVANCED_FACE('',(#1879),#1160,.F.);
#14848=ADVANCED_FACE('',(#1880),#1161,.F.);
#14849=ADVANCED_FACE('',(#1881),#1162,.T.);
#14850=ADVANCED_FACE('',(#1882),#1163,.T.);
#14851=ADVANCED_FACE('',(#1883),#14171,.T.);
#14852=ADVANCED_FACE('',(#1884),#14172,.T.);
#14853=ADVANCED_FACE('',(#1885),#14173,.T.);
#14854=ADVANCED_FACE('',(#1886),#14174,.T.);
#14855=ADVANCED_FACE('',(#1887),#14175,.T.);
#14856=ADVANCED_FACE('',(#1888),#14176,.T.);
#14857=ADVANCED_FACE('',(#1889),#14177,.T.);
#14858=ADVANCED_FACE('',(#1890),#1164,.T.);
#14859=ADVANCED_FACE('',(#1891),#14178,.T.);
#14860=ADVANCED_FACE('',(#1892),#1165,.F.);
#14861=ADVANCED_FACE('',(#1893),#14179,.T.);
#14862=ADVANCED_FACE('',(#1894),#1166,.T.);
#14863=ADVANCED_FACE('',(#1895),#14180,.T.);
#14864=ADVANCED_FACE('',(#1896),#14181,.F.);
#14865=ADVANCED_FACE('',(#1897),#14182,.F.);
#14866=ADVANCED_FACE('',(#1898),#14183,.F.);
#14867=ADVANCED_FACE('',(#1899),#14184,.F.);
#14868=ADVANCED_FACE('',(#1900),#1167,.F.);
#14869=ADVANCED_FACE('',(#1901,#1587),#14185,.F.);
#14870=ADVANCED_FACE('',(#1902,#1588),#14186,.T.);
#14871=ADVANCED_FACE('',(#1903),#14187,.F.);
#14872=ADVANCED_FACE('',(#1904),#14188,.F.);
#14873=ADVANCED_FACE('',(#1905),#14189,.F.);
#14874=ADVANCED_FACE('',(#1906),#1168,.T.);
#14875=ADVANCED_FACE('',(#1907),#14190,.F.);
#14876=ADVANCED_FACE('',(#1908),#14191,.F.);
#14877=ADVANCED_FACE('',(#1909),#1169,.F.);
#14878=ADVANCED_FACE('',(#1910,#1589),#14192,.F.);
#14879=ADVANCED_FACE('',(#1911,#1590),#14193,.T.);
#14880=ADVANCED_FACE('',(#1912),#14194,.F.);
#14881=ADVANCED_FACE('',(#1913),#14195,.F.);
#14882=ADVANCED_FACE('',(#1914),#14196,.F.);
#14883=ADVANCED_FACE('',(#1915),#1170,.T.);
#14884=ADVANCED_FACE('',(#1916),#14197,.F.);
#14885=ADVANCED_FACE('',(#1917),#14198,.F.);
#14886=ADVANCED_FACE('',(#1918),#14199,.T.);
#14887=ADVANCED_FACE('',(#1919),#14200,.T.);
#14888=ADVANCED_FACE('',(#1920),#1171,.F.);
#14889=ADVANCED_FACE('',(#1921),#14201,.T.);
#14890=ADVANCED_FACE('',(#1922),#14202,.T.);
#14891=ADVANCED_FACE('',(#1923),#14203,.T.);
#14892=ADVANCED_FACE('',(#1924),#1172,.F.);
#14893=ADVANCED_FACE('',(#1925),#14204,.T.);
#14894=ADVANCED_FACE('',(#1926),#14205,.T.);
#14895=ADVANCED_FACE('',(#1927),#14206,.T.);
#14896=ADVANCED_FACE('',(#1928),#14207,.T.);
#14897=ADVANCED_FACE('',(#1929),#14208,.T.);
#14898=ADVANCED_FACE('',(#1930),#14209,.F.);
#14899=ADVANCED_FACE('',(#1931),#14210,.T.);
#14900=ADVANCED_FACE('',(#1932),#1173,.F.);
#14901=ADVANCED_FACE('',(#1933),#1174,.F.);
#14902=ADVANCED_FACE('',(#1934),#1175,.T.);
#14903=ADVANCED_FACE('',(#1935,#1591),#14211,.F.);
#14904=ADVANCED_FACE('',(#1936,#1592),#14212,.T.);
#14905=ADVANCED_FACE('',(#1937),#14213,.F.);
#14906=ADVANCED_FACE('',(#1938),#14214,.F.);
#14907=ADVANCED_FACE('',(#1939),#14215,.F.);
#14908=ADVANCED_FACE('',(#1940),#14216,.F.);
#14909=ADVANCED_FACE('',(#1941),#1176,.F.);
#14910=ADVANCED_FACE('',(#1942),#1177,.F.);
#14911=ADVANCED_FACE('',(#1943),#1178,.T.);
#14912=ADVANCED_FACE('',(#1944,#1593),#14217,.F.);
#14913=ADVANCED_FACE('',(#1945,#1594),#14218,.T.);
#14914=ADVANCED_FACE('',(#1946),#14219,.F.);
#14915=ADVANCED_FACE('',(#1947),#14220,.F.);
#14916=ADVANCED_FACE('',(#1948),#14221,.F.);
#14917=ADVANCED_FACE('',(#1949),#14222,.F.);
#14918=ADVANCED_FACE('',(#1950),#639,.T.);
#14919=ADVANCED_FACE('',(#1951),#640,.T.);
#14920=ADVANCED_FACE('',(#1952),#1179,.T.);
#14921=ADVANCED_FACE('',(#1953),#1180,.T.);
#14922=ADVANCED_FACE('',(#1954),#1181,.T.);
#14923=ADVANCED_FACE('',(#1955),#14223,.F.);
#14924=ADVANCED_FACE('',(#1956),#14224,.T.);
#14925=ADVANCED_FACE('',(#1957),#574,.T.);
#14926=ADVANCED_FACE('',(#1958),#1182,.T.);
#14927=ADVANCED_FACE('',(#1959),#14225,.F.);
#14928=ADVANCED_FACE('',(#1960),#14226,.F.);
#14929=ADVANCED_FACE('',(#1961),#14227,.F.);
#14930=ADVANCED_FACE('',(#1962),#14228,.F.);
#14931=ADVANCED_FACE('',(#1963),#14229,.F.);
#14932=ADVANCED_FACE('',(#1964),#14230,.F.);
#14933=ADVANCED_FACE('',(#1965,#1595),#14231,.T.);
#14934=ADVANCED_FACE('',(#1966),#14232,.F.);
#14935=ADVANCED_FACE('',(#1967),#575,.T.);
#14936=ADVANCED_FACE('',(#1968),#576,.T.);
#14937=ADVANCED_FACE('',(#1969),#577,.T.);
#14938=ADVANCED_FACE('',(#1970),#578,.T.);
#14939=ADVANCED_FACE('',(#1971),#579,.T.);
#14940=ADVANCED_FACE('',(#1972),#580,.T.);
#14941=ADVANCED_FACE('',(#1973),#14233,.F.);
#14942=ADVANCED_FACE('',(#1974),#581,.T.);
#14943=ADVANCED_FACE('',(#1975),#1183,.T.);
#14944=ADVANCED_FACE('',(#1976),#14234,.F.);
#14945=ADVANCED_FACE('',(#1977),#14235,.F.);
#14946=ADVANCED_FACE('',(#1978),#14236,.F.);
#14947=ADVANCED_FACE('',(#1979),#14237,.F.);
#14948=ADVANCED_FACE('',(#1980),#14238,.F.);
#14949=ADVANCED_FACE('',(#1981),#14239,.F.);
#14950=ADVANCED_FACE('',(#1982,#1596),#14240,.T.);
#14951=ADVANCED_FACE('',(#1983),#14241,.F.);
#14952=ADVANCED_FACE('',(#1984),#582,.T.);
#14953=ADVANCED_FACE('',(#1985),#583,.T.);
#14954=ADVANCED_FACE('',(#1986),#584,.T.);
#14955=ADVANCED_FACE('',(#1987),#585,.T.);
#14956=ADVANCED_FACE('',(#1988),#586,.T.);
#14957=ADVANCED_FACE('',(#1989),#587,.T.);
#14958=ADVANCED_FACE('',(#1990),#14242,.F.);
#14959=ADVANCED_FACE('',(#1991),#1184,.F.);
#14960=ADVANCED_FACE('',(#1992),#588,.F.);
#14961=ADVANCED_FACE('',(#1993),#589,.F.);
#14962=ADVANCED_FACE('',(#1994),#1185,.F.);
#14963=ADVANCED_FACE('',(#1995),#14243,.T.);
#14964=ADVANCED_FACE('',(#1996),#14244,.T.);
#14965=ADVANCED_FACE('',(#1997),#14245,.F.);
#14966=ADVANCED_FACE('',(#1998),#14246,.T.);
#14967=ADVANCED_FACE('',(#1999),#14247,.T.);
#14968=ADVANCED_FACE('',(#2000),#14248,.T.);
#14969=ADVANCED_FACE('',(#2001,#1597),#14249,.F.);
#14970=ADVANCED_FACE('',(#2002,#1598),#14250,.T.);
#14971=ADVANCED_FACE('',(#2003),#590,.T.);
#14972=ADVANCED_FACE('',(#2004),#591,.T.);
#14973=ADVANCED_FACE('',(#2005),#592,.T.);
#14974=ADVANCED_FACE('',(#2006),#593,.T.);
#14975=ADVANCED_FACE('',(#2007),#594,.T.);
#14976=ADVANCED_FACE('',(#2008),#595,.T.);
#14977=ADVANCED_FACE('',(#2009),#596,.T.);
#14978=ADVANCED_FACE('',(#2010),#597,.T.);
#14979=ADVANCED_FACE('',(#2011),#598,.T.);
#14980=ADVANCED_FACE('',(#2012),#599,.T.);
#14981=ADVANCED_FACE('',(#2013),#600,.T.);
#14982=ADVANCED_FACE('',(#2014),#601,.T.);
#14983=ADVANCED_FACE('',(#2015),#1186,.T.);
#14984=ADVANCED_FACE('',(#2016),#1187,.T.);
#14985=ADVANCED_FACE('',(#2017),#1188,.T.);
#14986=ADVANCED_FACE('',(#2018),#1189,.T.);
#14987=ADVANCED_FACE('',(#2019),#1190,.T.);
#14988=ADVANCED_FACE('',(#2020),#1191,.T.);
#14989=ADVANCED_FACE('',(#2021),#1192,.T.);
#14990=ADVANCED_FACE('',(#2022),#1193,.T.);
#14991=ADVANCED_FACE('',(#2023),#1194,.T.);
#14992=ADVANCED_FACE('',(#2024),#1195,.T.);
#14993=ADVANCED_FACE('',(#2025),#1196,.T.);
#14994=ADVANCED_FACE('',(#2026),#1197,.T.);
#14995=ADVANCED_FACE('',(#2027),#1198,.T.);
#14996=ADVANCED_FACE('',(#2028),#1199,.T.);
#14997=ADVANCED_FACE('',(#2029),#1200,.T.);
#14998=ADVANCED_FACE('',(#2030),#1201,.T.);
#14999=ADVANCED_FACE('',(#2031),#1202,.T.);
#15000=ADVANCED_FACE('',(#2032),#1203,.T.);
#15001=ADVANCED_FACE('',(#2033),#1204,.T.);
#15002=ADVANCED_FACE('',(#2034),#1205,.T.);
#15003=ADVANCED_FACE('',(#2035),#1206,.T.);
#15004=ADVANCED_FACE('',(#2036),#1207,.T.);
#15005=ADVANCED_FACE('',(#2037),#1208,.T.);
#15006=ADVANCED_FACE('',(#2038),#1209,.T.);
#15007=ADVANCED_FACE('',(#2039),#1210,.T.);
#15008=ADVANCED_FACE('',(#2040),#1211,.T.);
#15009=ADVANCED_FACE('',(#2041),#1212,.T.);
#15010=ADVANCED_FACE('',(#2042),#1213,.T.);
#15011=ADVANCED_FACE('',(#2043),#1214,.T.);
#15012=ADVANCED_FACE('',(#2044),#1215,.T.);
#15013=ADVANCED_FACE('',(#2045),#1216,.T.);
#15014=ADVANCED_FACE('',(#2046),#1217,.T.);
#15015=ADVANCED_FACE('',(#2047),#1218,.T.);
#15016=ADVANCED_FACE('',(#2048),#1219,.T.);
#15017=ADVANCED_FACE('',(#2049),#1220,.T.);
#15018=ADVANCED_FACE('',(#2050),#1221,.T.);
#15019=ADVANCED_FACE('',(#2051),#1222,.T.);
#15020=ADVANCED_FACE('',(#2052),#1223,.T.);
#15021=ADVANCED_FACE('',(#2053),#1224,.T.);
#15022=ADVANCED_FACE('',(#2054),#1225,.T.);
#15023=ADVANCED_FACE('',(#2055),#1226,.T.);
#15024=ADVANCED_FACE('',(#2056),#1227,.T.);
#15025=ADVANCED_FACE('',(#2057),#1228,.T.);
#15026=ADVANCED_FACE('',(#2058),#641,.T.);
#15027=ADVANCED_FACE('',(#2059),#642,.T.);
#15028=ADVANCED_FACE('',(#2060),#1229,.F.);
#15029=ADVANCED_FACE('',(#2061),#1230,.T.);
#15030=ADVANCED_FACE('',(#2062),#602,.T.);
#15031=ADVANCED_FACE('',(#2063),#1231,.T.);
#15032=ADVANCED_FACE('',(#2064,#1599),#14251,.F.);
#15033=ADVANCED_FACE('',(#2065,#1600),#14252,.T.);
#15034=ADVANCED_FACE('',(#2066),#14253,.T.);
#15035=ADVANCED_FACE('',(#2067),#14254,.T.);
#15036=ADVANCED_FACE('',(#2068),#299,.T.);
#15037=ADVANCED_FACE('',(#2069),#1232,.T.);
#15038=ADVANCED_FACE('',(#2070),#300,.T.);
#15039=ADVANCED_FACE('',(#2071),#301,.F.);
#15040=ADVANCED_FACE('',(#2072),#302,.F.);
#15041=ADVANCED_FACE('',(#2073),#303,.F.);
#15042=ADVANCED_FACE('',(#2074),#304,.F.);
#15043=ADVANCED_FACE('',(#2075),#305,.F.);
#15044=ADVANCED_FACE('',(#2076),#306,.F.);
#15045=ADVANCED_FACE('',(#2077),#307,.T.);
#15046=ADVANCED_FACE('',(#2078),#308,.T.);
#15047=ADVANCED_FACE('',(#2079),#309,.T.);
#15048=ADVANCED_FACE('',(#2080),#310,.T.);
#15049=ADVANCED_FACE('',(#2081),#311,.T.);
#15050=ADVANCED_FACE('',(#2082),#312,.T.);
#15051=ADVANCED_FACE('',(#2083),#313,.T.);
#15052=ADVANCED_FACE('',(#2084),#314,.T.);
#15053=ADVANCED_FACE('',(#2085),#1233,.F.);
#15054=ADVANCED_FACE('',(#2086),#1234,.F.);
#15055=ADVANCED_FACE('',(#2087),#1235,.F.);
#15056=ADVANCED_FACE('',(#2088),#1236,.F.);
#15057=ADVANCED_FACE('',(#2089),#1237,.F.);
#15058=ADVANCED_FACE('',(#2090),#1238,.F.);
#15059=ADVANCED_FACE('',(#2091),#1239,.F.);
#15060=ADVANCED_FACE('',(#2092),#1240,.F.);
#15061=ADVANCED_FACE('',(#2093),#1241,.F.);
#15062=ADVANCED_FACE('',(#2094),#1242,.F.);
#15063=ADVANCED_FACE('',(#2095),#1243,.F.);
#15064=ADVANCED_FACE('',(#2096),#603,.T.);
#15065=ADVANCED_FACE('',(#2097),#1244,.T.);
#15066=ADVANCED_FACE('',(#2098),#604,.T.);
#15067=ADVANCED_FACE('',(#2099),#1245,.F.);
#15068=ADVANCED_FACE('',(#2100),#605,.T.);
#15069=ADVANCED_FACE('',(#2101),#14255,.F.);
#15070=ADVANCED_FACE('',(#2102),#14256,.F.);
#15071=ADVANCED_FACE('',(#2103,#1601),#14257,.T.);
#15072=ADVANCED_FACE('',(#2104,#1602),#14258,.F.);
#15073=ADVANCED_FACE('',(#2105),#14259,.F.);
#15074=ADVANCED_FACE('',(#2106),#14260,.F.);
#15075=ADVANCED_FACE('',(#2107),#14261,.F.);
#15076=ADVANCED_FACE('',(#2108),#14262,.F.);
#15077=ADVANCED_FACE('',(#2109),#606,.T.);
#15078=ADVANCED_FACE('',(#2110),#607,.T.);
#15079=ADVANCED_FACE('',(#2111),#608,.T.);
#15080=ADVANCED_FACE('',(#2112),#609,.T.);
#15081=ADVANCED_FACE('',(#2113),#610,.T.);
#15082=ADVANCED_FACE('',(#2114),#611,.T.);
#15083=ADVANCED_FACE('',(#2115),#612,.T.);
#15084=ADVANCED_FACE('',(#2116),#613,.T.);
#15085=ADVANCED_FACE('',(#2117),#614,.T.);
#15086=ADVANCED_FACE('',(#2118),#615,.T.);
#15087=ADVANCED_FACE('',(#2119),#616,.T.);
#15088=ADVANCED_FACE('',(#2120),#617,.T.);
#15089=ADVANCED_FACE('',(#2121),#315,.F.);
#15090=ADVANCED_FACE('',(#2122),#1246,.F.);
#15091=ADVANCED_FACE('',(#2123),#316,.F.);
#15092=ADVANCED_FACE('',(#2124),#1247,.T.);
#15093=ADVANCED_FACE('',(#2125),#14263,.T.);
#15094=ADVANCED_FACE('',(#2126),#1248,.T.);
#15095=ADVANCED_FACE('',(#2127),#1249,.F.);
#15096=ADVANCED_FACE('',(#2128,#1603),#14264,.F.);
#15097=ADVANCED_FACE('',(#2129,#1604),#14265,.F.);
#15098=ADVANCED_FACE('',(#2130),#14266,.F.);
#15099=ADVANCED_FACE('',(#2131),#14267,.F.);
#15100=ADVANCED_FACE('',(#2132),#14268,.F.);
#15101=ADVANCED_FACE('',(#2133),#14269,.F.);
#15102=ADVANCED_FACE('',(#2134),#14270,.F.);
#15103=ADVANCED_FACE('',(#2135),#14271,.T.);
#15104=ADVANCED_FACE('',(#2136),#1250,.F.);
#15105=ADVANCED_FACE('',(#2137,#1605),#14272,.T.);
#15106=ADVANCED_FACE('',(#2138,#1606),#14273,.F.);
#15107=ADVANCED_FACE('',(#2139),#14274,.F.);
#15108=ADVANCED_FACE('',(#2140),#14275,.F.);
#15109=ADVANCED_FACE('',(#2141),#14276,.F.);
#15110=ADVANCED_FACE('',(#2142),#14277,.F.);
#15111=ADVANCED_FACE('',(#2143),#1251,.F.);
#15112=ADVANCED_FACE('',(#2144),#14278,.F.);
#15113=ADVANCED_FACE('',(#2145),#1252,.F.);
#15114=ADVANCED_FACE('',(#2146,#1607),#14279,.T.);
#15115=ADVANCED_FACE('',(#2147,#1608),#14280,.F.);
#15116=ADVANCED_FACE('',(#2148),#14281,.F.);
#15117=ADVANCED_FACE('',(#2149),#14282,.F.);
#15118=ADVANCED_FACE('',(#2150),#14283,.F.);
#15119=ADVANCED_FACE('',(#2151),#14284,.F.);
#15120=ADVANCED_FACE('',(#2152),#1253,.F.);
#15121=ADVANCED_FACE('',(#2153),#14285,.F.);
#15122=ADVANCED_FACE('',(#2154),#1254,.F.);
#15123=ADVANCED_FACE('',(#2155),#1255,.F.);
#15124=ADVANCED_FACE('',(#2156),#1256,.F.);
#15125=ADVANCED_FACE('',(#2157),#1257,.F.);
#15126=ADVANCED_FACE('',(#2158),#1258,.F.);
#15127=ADVANCED_FACE('',(#2159,#1609,#1610,#1611,#1612,#1613),#14286,.F.);
#15128=ADVANCED_FACE('',(#2160,#1614,#1615,#1616,#1617,#1618),#14287,.T.);
#15129=ADVANCED_FACE('',(#2161),#14288,.F.);
#15130=ADVANCED_FACE('',(#2162),#14289,.F.);
#15131=ADVANCED_FACE('',(#2163),#14290,.F.);
#15132=ADVANCED_FACE('',(#2164),#14291,.F.);
#15133=ADVANCED_FACE('',(#2165),#14292,.F.);
#15134=ADVANCED_FACE('',(#2166),#14293,.F.);
#15135=ADVANCED_FACE('',(#2167),#14294,.F.);
#15136=ADVANCED_FACE('',(#2168),#14295,.F.);
#15137=ADVANCED_FACE('',(#2169),#14296,.F.);
#15138=ADVANCED_FACE('',(#2170),#14297,.F.);
#15139=ADVANCED_FACE('',(#2171),#14298,.F.);
#15140=ADVANCED_FACE('',(#2172),#14299,.F.);
#15141=ADVANCED_FACE('',(#2173),#14300,.F.);
#15142=ADVANCED_FACE('',(#2174),#14301,.T.);
#15143=ADVANCED_FACE('',(#2175),#14302,.F.);
#15144=ADVANCED_FACE('',(#2176),#14303,.F.);
#15145=ADVANCED_FACE('',(#2177),#14304,.F.);
#15146=ADVANCED_FACE('',(#2178),#14305,.F.);
#15147=ADVANCED_FACE('',(#2179),#14306,.T.);
#15148=ADVANCED_FACE('',(#2180),#14307,.F.);
#15149=ADVANCED_FACE('',(#2181),#14308,.F.);
#15150=ADVANCED_FACE('',(#2182),#14309,.F.);
#15151=ADVANCED_FACE('',(#2183),#14310,.F.);
#15152=ADVANCED_FACE('',(#2184),#14311,.F.);
#15153=ADVANCED_FACE('',(#2185),#14312,.F.);
#15154=ADVANCED_FACE('',(#2186),#14313,.F.);
#15155=ADVANCED_FACE('',(#2187),#14314,.T.);
#15156=ADVANCED_FACE('',(#2188),#14315,.F.);
#15157=ADVANCED_FACE('',(#2189),#1259,.F.);
#15158=ADVANCED_FACE('',(#2190),#1260,.F.);
#15159=ADVANCED_FACE('',(#2191),#1261,.F.);
#15160=ADVANCED_FACE('',(#2192,#1619,#1620,#1621),#14316,.T.);
#15161=ADVANCED_FACE('',(#2193,#1622,#1623,#1624),#14317,.F.);
#15162=ADVANCED_FACE('',(#2194),#14318,.F.);
#15163=ADVANCED_FACE('',(#2195),#14319,.F.);
#15164=ADVANCED_FACE('',(#2196),#14320,.F.);
#15165=ADVANCED_FACE('',(#2197),#14321,.F.);
#15166=ADVANCED_FACE('',(#2198),#1262,.F.);
#15167=ADVANCED_FACE('',(#2199),#1263,.F.);
#15168=ADVANCED_FACE('',(#2200),#1264,.F.);
#15169=ADVANCED_FACE('',(#2201,#1625,#1626,#1627),#14322,.T.);
#15170=ADVANCED_FACE('',(#2202,#1628,#1629,#1630),#14323,.F.);
#15171=ADVANCED_FACE('',(#2203),#14324,.F.);
#15172=ADVANCED_FACE('',(#2204),#14325,.F.);
#15173=ADVANCED_FACE('',(#2205),#14326,.F.);
#15174=ADVANCED_FACE('',(#2206),#14327,.F.);
#15175=ADVANCED_FACE('',(#2207),#1265,.F.);
#15176=ADVANCED_FACE('',(#2208),#1266,.F.);
#15177=ADVANCED_FACE('',(#2209),#1267,.F.);
#15178=ADVANCED_FACE('',(#2210,#1631,#1632,#1633),#14328,.T.);
#15179=ADVANCED_FACE('',(#2211,#1634,#1635,#1636),#14329,.F.);
#15180=ADVANCED_FACE('',(#2212),#14330,.F.);
#15181=ADVANCED_FACE('',(#2213),#14331,.F.);
#15182=ADVANCED_FACE('',(#2214),#14332,.F.);
#15183=ADVANCED_FACE('',(#2215),#14333,.F.);
#15184=ADVANCED_FACE('',(#2216),#1268,.F.);
#15185=ADVANCED_FACE('',(#2217),#1269,.F.);
#15186=ADVANCED_FACE('',(#2218),#1270,.F.);
#15187=ADVANCED_FACE('',(#2219,#1637,#1638,#1639),#14334,.T.);
#15188=ADVANCED_FACE('',(#2220,#1640,#1641,#1642),#14335,.F.);
#15189=ADVANCED_FACE('',(#2221),#14336,.F.);
#15190=ADVANCED_FACE('',(#2222),#14337,.F.);
#15191=ADVANCED_FACE('',(#2223),#14338,.F.);
#15192=ADVANCED_FACE('',(#2224),#14339,.F.);
#15193=ADVANCED_FACE('',(#2225),#14340,.F.);
#15194=ADVANCED_FACE('',(#2226),#14341,.F.);
#15195=ADVANCED_FACE('',(#2227),#14342,.F.);
#15196=ADVANCED_FACE('',(#2228),#14343,.F.);
#15197=ADVANCED_FACE('',(#2229),#14344,.F.);
#15198=ADVANCED_FACE('',(#2230),#14345,.T.);
#15199=ADVANCED_FACE('',(#2231),#14346,.F.);
#15200=ADVANCED_FACE('',(#2232),#14347,.F.);
#15201=ADVANCED_FACE('',(#2233),#14348,.F.);
#15202=ADVANCED_FACE('',(#2234),#14349,.F.);
#15203=ADVANCED_FACE('',(#2235),#14350,.T.);
#15204=ADVANCED_FACE('',(#2236),#14351,.F.);
#15205=ADVANCED_FACE('',(#2237),#14352,.T.);
#15206=ADVANCED_FACE('',(#2238),#14353,.T.);
#15207=ADVANCED_FACE('',(#2239),#14354,.T.);
#15208=ADVANCED_FACE('',(#2240),#14355,.T.);
#15209=ADVANCED_FACE('',(#2241),#14356,.F.);
#15210=ADVANCED_FACE('',(#2242),#14357,.T.);
#15211=ADVANCED_FACE('',(#2243),#14358,.T.);
#15212=ADVANCED_FACE('',(#2244),#14359,.T.);
#15213=ADVANCED_FACE('',(#2245),#14360,.T.);
#15214=ADVANCED_FACE('',(#2246),#14361,.T.);
#15215=ADVANCED_FACE('',(#2247),#14362,.F.);
#15216=ADVANCED_FACE('',(#2248),#14363,.T.);
#15217=ADVANCED_FACE('',(#2249),#14364,.T.);
#15218=ADVANCED_FACE('',(#2250),#14365,.T.);
#15219=ADVANCED_FACE('',(#2251),#14366,.T.);
#15220=ADVANCED_FACE('',(#2252),#14367,.T.);
#15221=ADVANCED_FACE('',(#2253),#14368,.F.);
#15222=ADVANCED_FACE('',(#2254),#14369,.T.);
#15223=ADVANCED_FACE('',(#2255),#1271,.F.);
#15224=ADVANCED_FACE('',(#2256),#1272,.F.);
#15225=ADVANCED_FACE('',(#2257),#1273,.F.);
#15226=ADVANCED_FACE('',(#2258),#1274,.F.);
#15227=ADVANCED_FACE('',(#2259,#1643,#1644,#1645,#1646),#14370,.F.);
#15228=ADVANCED_FACE('',(#2260,#1647,#1648,#1649,#1650),#14371,.T.);
#15229=ADVANCED_FACE('',(#2261),#14372,.F.);
#15230=ADVANCED_FACE('',(#2262),#14373,.F.);
#15231=ADVANCED_FACE('',(#2263),#14374,.F.);
#15232=ADVANCED_FACE('',(#2264),#14375,.F.);
#15233=ADVANCED_FACE('',(#2265),#1275,.F.);
#15234=ADVANCED_FACE('',(#2266),#1276,.F.);
#15235=ADVANCED_FACE('',(#2267),#1277,.F.);
#15236=ADVANCED_FACE('',(#2268),#1278,.F.);
#15237=ADVANCED_FACE('',(#2269),#1279,.F.);
#15238=ADVANCED_FACE('',(#2270),#1280,.F.);
#15239=ADVANCED_FACE('',(#2271),#14376,.T.);
#15240=ADVANCED_FACE('',(#2272),#14377,.T.);
#15241=ADVANCED_FACE('',(#2273),#14378,.T.);
#15242=ADVANCED_FACE('',(#2274),#14379,.T.);
#15243=ADVANCED_FACE('',(#2275,#1651,#1652,#1653,#1654,#1655,#1656),#14380,
 .F.);
#15244=ADVANCED_FACE('',(#2276,#1657,#1658,#1659,#1660,#1661,#1662),#14381,
 .T.);
#15245=ADVANCED_FACE('',(#2277),#14382,.F.);
#15246=ADVANCED_FACE('',(#2278),#14383,.F.);
#15247=ADVANCED_FACE('',(#2279),#14384,.F.);
#15248=ADVANCED_FACE('',(#2280),#14385,.F.);
#15249=ADVANCED_FACE('',(#2281),#14386,.F.);
#15250=ADVANCED_FACE('',(#2282),#14387,.F.);
#15251=ADVANCED_FACE('',(#2283),#14388,.F.);
#15252=ADVANCED_FACE('',(#2284),#14389,.F.);
#15253=ADVANCED_FACE('',(#2285),#14390,.T.);
#15254=ADVANCED_FACE('',(#2286),#14391,.F.);
#15255=ADVANCED_FACE('',(#2287),#14392,.F.);
#15256=ADVANCED_FACE('',(#2288),#14393,.F.);
#15257=ADVANCED_FACE('',(#2289),#14394,.F.);
#15258=ADVANCED_FACE('',(#2290),#14395,.F.);
#15259=ADVANCED_FACE('',(#2291),#14396,.F.);
#15260=ADVANCED_FACE('',(#2292),#14397,.F.);
#15261=ADVANCED_FACE('',(#2293),#14398,.F.);
#15262=ADVANCED_FACE('',(#2294),#14399,.T.);
#15263=ADVANCED_FACE('',(#2295),#14400,.F.);
#15264=ADVANCED_FACE('',(#2296),#14401,.F.);
#15265=ADVANCED_FACE('',(#2297),#14402,.F.);
#15266=ADVANCED_FACE('',(#2298),#14403,.F.);
#15267=ADVANCED_FACE('',(#2299),#14404,.F.);
#15268=ADVANCED_FACE('',(#2300),#14405,.F.);
#15269=ADVANCED_FACE('',(#2301),#14406,.F.);
#15270=ADVANCED_FACE('',(#2302),#14407,.F.);
#15271=ADVANCED_FACE('',(#2303),#14408,.T.);
#15272=ADVANCED_FACE('',(#2304),#14409,.T.);
#15273=ADVANCED_FACE('',(#2305),#14410,.T.);
#15274=ADVANCED_FACE('',(#2306),#14411,.T.);
#15275=ADVANCED_FACE('',(#2307),#14412,.T.);
#15276=ADVANCED_FACE('',(#2308),#14413,.T.);
#15277=ADVANCED_FACE('',(#2309),#14414,.T.);
#15278=ADVANCED_FACE('',(#2310),#14415,.T.);
#15279=ADVANCED_FACE('',(#2311),#14416,.T.);
#15280=ADVANCED_FACE('',(#2312),#14417,.F.);
#15281=ADVANCED_FACE('',(#2313),#14418,.T.);
#15282=ADVANCED_FACE('',(#2314),#14419,.T.);
#15283=ADVANCED_FACE('',(#2315),#14420,.T.);
#15284=ADVANCED_FACE('',(#2316),#14421,.T.);
#15285=ADVANCED_FACE('',(#2317),#14422,.T.);
#15286=ADVANCED_FACE('',(#2318),#14423,.T.);
#15287=ADVANCED_FACE('',(#2319),#14424,.T.);
#15288=ADVANCED_FACE('',(#2320),#14425,.T.);
#15289=ADVANCED_FACE('',(#2321),#14426,.F.);
#15290=ADVANCED_FACE('',(#2322),#14427,.T.);
#15291=ADVANCED_FACE('',(#2323),#14428,.T.);
#15292=ADVANCED_FACE('',(#2324),#14429,.T.);
#15293=ADVANCED_FACE('',(#2325),#14430,.T.);
#15294=ADVANCED_FACE('',(#2326),#14431,.T.);
#15295=ADVANCED_FACE('',(#2327),#14432,.T.);
#15296=ADVANCED_FACE('',(#2328),#14433,.T.);
#15297=ADVANCED_FACE('',(#2329),#14434,.T.);
#15298=ADVANCED_FACE('',(#2330),#14435,.F.);
#15299=ADVANCED_FACE('',(#2331),#14436,.T.);
#15300=ADVANCED_FACE('',(#2332),#14437,.T.);
#15301=ADVANCED_FACE('',(#2333),#14438,.T.);
#15302=ADVANCED_FACE('',(#2334),#14439,.T.);
#15303=ADVANCED_FACE('',(#2335),#14440,.T.);
#15304=ADVANCED_FACE('',(#2336),#14441,.T.);
#15305=ADVANCED_FACE('',(#2337),#14442,.T.);
#15306=ADVANCED_FACE('',(#2338),#14443,.T.);
#15307=ADVANCED_FACE('',(#2339),#14444,.F.);
#15308=ADVANCED_FACE('',(#2340),#14445,.T.);
#15309=ADVANCED_FACE('',(#2341),#14446,.T.);
#15310=ADVANCED_FACE('',(#2342),#14447,.T.);
#15311=ADVANCED_FACE('',(#2343),#14448,.T.);
#15312=ADVANCED_FACE('',(#2344),#14449,.T.);
#15313=ADVANCED_FACE('',(#2345),#14450,.T.);
#15314=ADVANCED_FACE('',(#2346),#14451,.T.);
#15315=ADVANCED_FACE('',(#2347),#14452,.T.);
#15316=ADVANCED_FACE('',(#2348),#14453,.F.);
#15317=ADVANCED_FACE('',(#2349),#14454,.F.);
#15318=ADVANCED_FACE('',(#2350),#14455,.F.);
#15319=ADVANCED_FACE('',(#2351),#14456,.F.);
#15320=ADVANCED_FACE('',(#2352),#14457,.F.);
#15321=ADVANCED_FACE('',(#2353),#14458,.F.);
#15322=ADVANCED_FACE('',(#2354),#14459,.F.);
#15323=ADVANCED_FACE('',(#2355),#14460,.F.);
#15324=ADVANCED_FACE('',(#2356),#14461,.F.);
#15325=ADVANCED_FACE('',(#2357),#14462,.T.);
#15326=ADVANCED_FACE('',(#2358),#14463,.F.);
#15327=ADVANCED_FACE('',(#2359),#14464,.F.);
#15328=ADVANCED_FACE('',(#2360),#14465,.F.);
#15329=ADVANCED_FACE('',(#2361),#14466,.F.);
#15330=ADVANCED_FACE('',(#2362),#14467,.F.);
#15331=ADVANCED_FACE('',(#2363),#14468,.F.);
#15332=ADVANCED_FACE('',(#2364),#14469,.F.);
#15333=ADVANCED_FACE('',(#2365),#14470,.F.);
#15334=ADVANCED_FACE('',(#2366),#14471,.T.);
#15335=ADVANCED_FACE('',(#2367),#14472,.F.);
#15336=ADVANCED_FACE('',(#2368),#14473,.F.);
#15337=ADVANCED_FACE('',(#2369),#14474,.F.);
#15338=ADVANCED_FACE('',(#2370),#14475,.F.);
#15339=ADVANCED_FACE('',(#2371),#14476,.F.);
#15340=ADVANCED_FACE('',(#2372),#14477,.F.);
#15341=ADVANCED_FACE('',(#2373),#14478,.F.);
#15342=ADVANCED_FACE('',(#2374),#14479,.F.);
#15343=ADVANCED_FACE('',(#2375),#14480,.T.);
#15344=ADVANCED_FACE('',(#2376),#1281,.F.);
#15345=ADVANCED_FACE('',(#2377),#1282,.F.);
#15346=ADVANCED_FACE('',(#2378),#1283,.F.);
#15347=ADVANCED_FACE('',(#2379),#1284,.F.);
#15348=ADVANCED_FACE('',(#2380,#1663,#1664,#1665,#1666),#14481,.F.);
#15349=ADVANCED_FACE('',(#2381,#1667,#1668,#1669,#1670),#14482,.T.);
#15350=ADVANCED_FACE('',(#2382),#14483,.F.);
#15351=ADVANCED_FACE('',(#2383),#14484,.F.);
#15352=ADVANCED_FACE('',(#2384),#14485,.F.);
#15353=ADVANCED_FACE('',(#2385),#14486,.F.);
#15354=ADVANCED_FACE('',(#2386),#14487,.F.);
#15355=ADVANCED_FACE('',(#2387),#14488,.F.);
#15356=ADVANCED_FACE('',(#2388),#14489,.F.);
#15357=ADVANCED_FACE('',(#2389),#14490,.F.);
#15358=ADVANCED_FACE('',(#2390),#14491,.T.);
#15359=ADVANCED_FACE('',(#2391),#14492,.F.);
#15360=ADVANCED_FACE('',(#2392),#14493,.F.);
#15361=ADVANCED_FACE('',(#2393),#14494,.F.);
#15362=ADVANCED_FACE('',(#2394),#14495,.F.);
#15363=ADVANCED_FACE('',(#2395),#14496,.F.);
#15364=ADVANCED_FACE('',(#2396),#14497,.T.);
#15365=ADVANCED_FACE('',(#2397),#14498,.F.);
#15366=ADVANCED_FACE('',(#2398),#14499,.F.);
#15367=ADVANCED_FACE('',(#2399),#14500,.F.);
#15368=ADVANCED_FACE('',(#2400),#14501,.F.);
#15369=ADVANCED_FACE('',(#2401),#14502,.F.);
#15370=ADVANCED_FACE('',(#2402),#14503,.T.);
#15371=ADVANCED_FACE('',(#2403),#14504,.F.);
#15372=ADVANCED_FACE('',(#2404),#14505,.F.);
#15373=ADVANCED_FACE('',(#2405),#14506,.F.);
#15374=ADVANCED_FACE('',(#2406),#14507,.F.);
#15375=ADVANCED_FACE('',(#2407),#14508,.F.);
#15376=ADVANCED_FACE('',(#2408),#14509,.T.);
#15377=ADVANCED_FACE('',(#2409),#14510,.F.);
#15378=ADVANCED_FACE('',(#2410),#14511,.F.);
#15379=ADVANCED_FACE('',(#2411),#14512,.F.);
#15380=ADVANCED_FACE('',(#2412),#14513,.F.);
#15381=ADVANCED_FACE('',(#2413),#14514,.F.);
#15382=ADVANCED_FACE('',(#2414),#14515,.T.);
#15383=ADVANCED_FACE('',(#2415),#14516,.F.);
#15384=ADVANCED_FACE('',(#2416),#14517,.F.);
#15385=ADVANCED_FACE('',(#2417),#14518,.F.);
#15386=ADVANCED_FACE('',(#2418),#14519,.F.);
#15387=ADVANCED_FACE('',(#2419),#14520,.F.);
#15388=ADVANCED_FACE('',(#2420),#14521,.T.);
#15389=ADVANCED_FACE('',(#2421),#14522,.F.);
#15390=ADVANCED_FACE('',(#2422),#14523,.F.);
#15391=ADVANCED_FACE('',(#2423),#14524,.F.);
#15392=ADVANCED_FACE('',(#2424),#14525,.F.);
#15393=ADVANCED_FACE('',(#2425),#14526,.F.);
#15394=ADVANCED_FACE('',(#2426),#14527,.T.);
#15395=ADVANCED_FACE('',(#2427),#14528,.F.);
#15396=ADVANCED_FACE('',(#2428),#14529,.F.);
#15397=ADVANCED_FACE('',(#2429),#14530,.F.);
#15398=ADVANCED_FACE('',(#2430),#14531,.F.);
#15399=ADVANCED_FACE('',(#2431),#14532,.F.);
#15400=ADVANCED_FACE('',(#2432),#14533,.T.);
#15401=ADVANCED_FACE('',(#2433),#14534,.F.);
#15402=ADVANCED_FACE('',(#2434),#14535,.F.);
#15403=ADVANCED_FACE('',(#2435),#14536,.F.);
#15404=ADVANCED_FACE('',(#2436),#14537,.F.);
#15405=ADVANCED_FACE('',(#2437),#14538,.F.);
#15406=ADVANCED_FACE('',(#2438),#14539,.T.);
#15407=ADVANCED_FACE('',(#2439),#14540,.F.);
#15408=ADVANCED_FACE('',(#2440),#14541,.F.);
#15409=ADVANCED_FACE('',(#2441),#14542,.F.);
#15410=ADVANCED_FACE('',(#2442),#14543,.F.);
#15411=ADVANCED_FACE('',(#2443),#14544,.F.);
#15412=ADVANCED_FACE('',(#2444),#14545,.T.);
#15413=ADVANCED_FACE('',(#2445),#14546,.F.);
#15414=ADVANCED_FACE('',(#2446),#14547,.F.);
#15415=ADVANCED_FACE('',(#2447),#14548,.F.);
#15416=ADVANCED_FACE('',(#2448),#14549,.F.);
#15417=ADVANCED_FACE('',(#2449),#14550,.F.);
#15418=ADVANCED_FACE('',(#2450),#14551,.T.);
#15419=ADVANCED_FACE('',(#2451),#14552,.F.);
#15420=ADVANCED_FACE('',(#2452),#14553,.F.);
#15421=ADVANCED_FACE('',(#2453),#14554,.F.);
#15422=ADVANCED_FACE('',(#2454),#14555,.F.);
#15423=ADVANCED_FACE('',(#2455),#14556,.F.);
#15424=ADVANCED_FACE('',(#2456),#14557,.T.);
#15425=ADVANCED_FACE('',(#2457),#14558,.F.);
#15426=ADVANCED_FACE('',(#2458),#14559,.F.);
#15427=ADVANCED_FACE('',(#2459),#14560,.F.);
#15428=ADVANCED_FACE('',(#2460),#14561,.F.);
#15429=ADVANCED_FACE('',(#2461),#14562,.F.);
#15430=ADVANCED_FACE('',(#2462),#14563,.T.);
#15431=ADVANCED_FACE('',(#2463),#14564,.F.);
#15432=ADVANCED_FACE('',(#2464),#14565,.F.);
#15433=ADVANCED_FACE('',(#2465),#14566,.F.);
#15434=ADVANCED_FACE('',(#2466),#14567,.F.);
#15435=ADVANCED_FACE('',(#2467),#14568,.F.);
#15436=ADVANCED_FACE('',(#2468),#14569,.T.);
#15437=ADVANCED_FACE('',(#2469),#14570,.F.);
#15438=ADVANCED_FACE('',(#2470),#14571,.F.);
#15439=ADVANCED_FACE('',(#2471),#14572,.F.);
#15440=ADVANCED_FACE('',(#2472),#14573,.F.);
#15441=ADVANCED_FACE('',(#2473),#14574,.F.);
#15442=ADVANCED_FACE('',(#2474),#14575,.T.);
#15443=ADVANCED_FACE('',(#2475),#14576,.F.);
#15444=ADVANCED_FACE('',(#2476),#14577,.F.);
#15445=ADVANCED_FACE('',(#2477),#14578,.F.);
#15446=ADVANCED_FACE('',(#2478),#14579,.F.);
#15447=ADVANCED_FACE('',(#2479),#14580,.F.);
#15448=ADVANCED_FACE('',(#2480),#14581,.T.);
#15449=ADVANCED_FACE('',(#2481),#14582,.F.);
#15450=ADVANCED_FACE('',(#2482),#14583,.F.);
#15451=ADVANCED_FACE('',(#2483),#14584,.F.);
#15452=ADVANCED_FACE('',(#2484),#14585,.F.);
#15453=ADVANCED_FACE('',(#2485),#14586,.F.);
#15454=ADVANCED_FACE('',(#2486),#14587,.T.);
#15455=ADVANCED_FACE('',(#2487),#14588,.F.);
#15456=ADVANCED_FACE('',(#2488),#14589,.F.);
#15457=ADVANCED_FACE('',(#2489),#14590,.F.);
#15458=ADVANCED_FACE('',(#2490),#14591,.F.);
#15459=ADVANCED_FACE('',(#2491),#14592,.F.);
#15460=ADVANCED_FACE('',(#2492),#14593,.T.);
#15461=ADVANCED_FACE('',(#2493),#14594,.F.);
#15462=ADVANCED_FACE('',(#2494),#14595,.F.);
#15463=ADVANCED_FACE('',(#2495),#14596,.F.);
#15464=ADVANCED_FACE('',(#2496),#14597,.F.);
#15465=ADVANCED_FACE('',(#2497),#14598,.F.);
#15466=ADVANCED_FACE('',(#2498),#14599,.F.);
#15467=ADVANCED_FACE('',(#2499),#14600,.T.);
#15468=ADVANCED_FACE('',(#2500),#14601,.F.);
#15469=ADVANCED_FACE('',(#2501),#14602,.F.);
#15470=ADVANCED_FACE('',(#2502),#14603,.F.);
#15471=ADVANCED_FACE('',(#2503),#14604,.F.);
#15472=ADVANCED_FACE('',(#2504),#14605,.F.);
#15473=ADVANCED_FACE('',(#2505),#14606,.T.);
#15474=ADVANCED_FACE('',(#2506),#14607,.F.);
#15475=ADVANCED_FACE('',(#2507),#14608,.F.);
#15476=ADVANCED_FACE('',(#2508),#14609,.F.);
#15477=ADVANCED_FACE('',(#2509),#14610,.F.);
#15478=ADVANCED_FACE('',(#2510),#14611,.T.);
#15479=ADVANCED_FACE('',(#2511),#14612,.F.);
#15480=ADVANCED_FACE('',(#2512),#14613,.F.);
#15481=ADVANCED_FACE('',(#2513),#14614,.F.);
#15482=ADVANCED_FACE('',(#2514),#14615,.F.);
#15483=ADVANCED_FACE('',(#2515),#14616,.F.);
#15484=ADVANCED_FACE('',(#2516),#14617,.T.);
#15485=ADVANCED_FACE('',(#2517),#14618,.F.);
#15486=ADVANCED_FACE('',(#2518),#643,.F.);
#15487=ADVANCED_FACE('',(#2519),#1285,.T.);
#15488=ADVANCED_FACE('',(#2520),#618,.T.);
#15489=ADVANCED_FACE('',(#2521),#1286,.T.);
#15490=ADVANCED_FACE('',(#2522,#1671),#14619,.T.);
#15491=ADVANCED_FACE('',(#2523),#14620,.F.);
#15492=ADVANCED_FACE('',(#2524),#14621,.T.);
#15493=ADVANCED_FACE('',(#2525),#14622,.T.);
#15494=ADVANCED_FACE('',(#2526),#14623,.T.);
#15495=ADVANCED_FACE('',(#2527),#14624,.T.);
#15496=ADVANCED_FACE('',(#2528),#14625,.T.);
#15497=ADVANCED_FACE('',(#2529),#14626,.T.);
#15498=ADVANCED_FACE('',(#2530),#14627,.F.);
#15499=ADVANCED_FACE('',(#2531),#619,.T.);
#15500=ADVANCED_FACE('',(#2532),#620,.T.);
#15501=ADVANCED_FACE('',(#2533),#621,.T.);
#15502=ADVANCED_FACE('',(#2534),#622,.T.);
#15503=ADVANCED_FACE('',(#2535),#623,.T.);
#15504=ADVANCED_FACE('',(#2536),#624,.T.);
#15505=ADVANCED_FACE('',(#2537),#14628,.F.);
#15506=ADVANCED_FACE('',(#2538),#14629,.F.);
#15507=ADVANCED_FACE('',(#2539),#14630,.F.);
#15508=ADVANCED_FACE('',(#2540),#14631,.F.);
#15509=ADVANCED_FACE('',(#2541),#14632,.F.);
#15510=ADVANCED_FACE('',(#2542),#14633,.F.);
#15511=ADVANCED_FACE('',(#2543),#1287,.T.);
#15512=ADVANCED_FACE('',(#2544),#1288,.F.);
#15513=ADVANCED_FACE('',(#2545,#1672),#14634,.F.);
#15514=ADVANCED_FACE('',(#2546,#1673),#14635,.F.);
#15515=ADVANCED_FACE('',(#2547),#1289,.F.);
#15516=ADVANCED_FACE('',(#2548),#625,.F.);
#15517=ADVANCED_FACE('',(#2549),#626,.F.);
#15518=ADVANCED_FACE('',(#2550),#1290,.F.);
#15519=ADVANCED_FACE('',(#2551),#14636,.T.);
#15520=ADVANCED_FACE('',(#2552),#14637,.T.);
#15521=ADVANCED_FACE('',(#2553),#14638,.F.);
#15522=ADVANCED_FACE('',(#2554),#14639,.T.);
#15523=ADVANCED_FACE('',(#2555),#14640,.T.);
#15524=ADVANCED_FACE('',(#2556),#14641,.T.);
#15525=ADVANCED_FACE('',(#2557,#1674),#14642,.F.);
#15526=ADVANCED_FACE('',(#2558,#1675),#14643,.T.);
#15527=ADVANCED_FACE('',(#2559),#627,.T.);
#15528=ADVANCED_FACE('',(#2560),#628,.T.);
#15529=ADVANCED_FACE('',(#2561),#629,.T.);
#15530=ADVANCED_FACE('',(#2562),#630,.T.);
#15531=ADVANCED_FACE('',(#2563),#631,.T.);
#15532=ADVANCED_FACE('',(#2564),#632,.T.);
#15533=ADVANCED_FACE('',(#2565),#633,.T.);
#15534=ADVANCED_FACE('',(#2566),#634,.T.);
#15535=ADVANCED_FACE('',(#2567),#635,.T.);
#15536=ADVANCED_FACE('',(#2568),#636,.T.);
#15537=ADVANCED_FACE('',(#2569),#637,.T.);
#15538=ADVANCED_FACE('',(#2570),#638,.T.);
#15539=CLOSED_SHELL('',(#14644,#14645,#14646,#14647,#14648,#14649,#14650,
#14651,#14652,#14653));
#15540=CLOSED_SHELL('',(#14654,#14655,#14656,#14657,#14658,#14659,#14660,
#14661));
#15541=CLOSED_SHELL('',(#14662,#14663,#14664,#14665,#14666,#14667,#14668,
#14669));
#15542=CLOSED_SHELL('',(#14670,#14671,#14672,#14673,#14674,#14675,#14676,
#14677,#14678,#14679,#14680,#14681));
#15543=CLOSED_SHELL('',(#14682,#14683,#14684,#14685,#14686,#14687,#14688,
#14689,#14690,#14691,#14692));
#15544=CLOSED_SHELL('',(#14693,#14694,#14695,#14696,#14697,#14698,#14699,
#14700,#14701,#14702,#14703));
#15545=CLOSED_SHELL('',(#14704,#14705,#14706,#14707,#14708,#14709));
#15546=CLOSED_SHELL('',(#14710,#14711,#14712,#14713,#14714,#14715));
#15547=CLOSED_SHELL('',(#14716,#14717,#14718,#14719,#14720,#14721));
#15548=CLOSED_SHELL('',(#14722,#14723,#14724,#14725,#14726,#14727,#14728,
#14729,#14730,#14731,#14732,#14733,#14734,#14735,#14736,#14737,#14738,#14739,
#14740,#14741,#14742,#14743,#14744,#14745));
#15549=CLOSED_SHELL('',(#14746,#14747,#14748,#14749));
#15550=CLOSED_SHELL('',(#14750,#14751,#14752,#14753));
#15551=CLOSED_SHELL('',(#14754,#14755,#14756,#14757,#14758,#14759,#14760,
#14761,#14762,#14763,#14764,#14765,#14766,#14767,#14768,#14769));
#15552=CLOSED_SHELL('',(#14770,#14771,#14772,#14773,#14774,#14775,#14776,
#14777));
#15553=CLOSED_SHELL('',(#14778,#14779,#14780,#14781,#14782,#14783,#14784,
#14785,#14786,#14787,#14788));
#15554=CLOSED_SHELL('',(#14789,#14790,#14791,#14792,#14793,#14794,#14795,
#14796,#14797,#14798,#14799));
#15555=CLOSED_SHELL('',(#14800,#14801,#14802,#14803,#14804,#14805,#14806,
#14807,#14808,#14809,#14810));
#15556=CLOSED_SHELL('',(#14811,#14812,#14813,#14814,#14815,#14816,#14817,
#14818,#14819));
#15557=CLOSED_SHELL('',(#14820,#14821,#14822,#14823,#14824,#14825,#14826,
#14827,#14828));
#15558=CLOSED_SHELL('',(#14829,#14830,#14831,#14832,#14833,#14834,#14835,
#14836,#14837));
#15559=CLOSED_SHELL('',(#14838,#14839,#14840,#14841,#14842,#14843,#14844,
#14845,#14846));
#15560=CLOSED_SHELL('',(#14847,#14848,#14849,#14850,#14851,#14852,#14853,
#14854,#14855,#14856,#14857,#14858,#14859,#14860,#14861,#14862,#14863,#14864,
#14865,#14866,#14867));
#15561=CLOSED_SHELL('',(#14868,#14869,#14870,#14871,#14872,#14873,#14874,
#14875,#14876));
#15562=CLOSED_SHELL('',(#14877,#14878,#14879,#14880,#14881,#14882,#14883,
#14884,#14885));
#15563=CLOSED_SHELL('',(#14886,#14887,#14888,#14889,#14890,#14891,#14892,
#14893,#14894,#14895,#14896,#14897,#14898,#14899));
#15564=CLOSED_SHELL('',(#14900,#14901,#14902,#14903,#14904,#14905,#14906,
#14907,#14908));
#15565=CLOSED_SHELL('',(#14909,#14910,#14911,#14912,#14913,#14914,#14915,
#14916,#14917));
#15566=CLOSED_SHELL('',(#14918,#14919,#14920,#14921,#14922,#14923,#14924));
#15567=CLOSED_SHELL('',(#14925,#14926,#14927,#14928,#14929,#14930,#14931,
#14932,#14933,#14934,#14935,#14936,#14937,#14938,#14939,#14940,#14941));
#15568=CLOSED_SHELL('',(#14942,#14943,#14944,#14945,#14946,#14947,#14948,
#14949,#14950,#14951,#14952,#14953,#14954,#14955,#14956,#14957,#14958));
#15569=CLOSED_SHELL('',(#14959,#14960,#14961,#14962,#14963,#14964,#14965,
#14966,#14967,#14968,#14969,#14970,#14971,#14972,#14973,#14974,#14975,#14976,
#14977,#14978,#14979,#14980,#14981,#14982));
#15570=CLOSED_SHELL('',(#14983,#14984,#14985,#14986,#14987,#14988,#14989,
#14990,#14991,#14992,#14993,#14994,#14995,#14996,#14997,#14998,#14999,#15000,
#15001,#15002,#15003,#15004,#15005,#15006,#15007,#15008,#15009,#15010,#15011,
#15012,#15013,#15014,#15015,#15016,#15017,#15018,#15019,#15020,#15021,#15022,
#15023,#15024,#15025,#15026,#15027,#15028,#15029,#15030,#15031,#15032,#15033,
#15034,#15035,#15036,#15037,#15038,#15039,#15040,#15041,#15042,#15043,#15044,
#15045,#15046,#15047,#15048,#15049,#15050,#15051,#15052));
#15571=CLOSED_SHELL('',(#15053,#15054,#15055,#15056,#15057,#15058,#15059,
#15060,#15061,#15062,#15063,#15064,#15065,#15066,#15067,#15068,#15069,#15070,
#15071,#15072,#15073,#15074,#15075,#15076,#15077,#15078,#15079,#15080,#15081,
#15082,#15083,#15084,#15085,#15086,#15087,#15088,#15089,#15090,#15091,#15092,
#15093));
#15572=CLOSED_SHELL('',(#15094,#15095,#15096,#15097));
#15573=CLOSED_SHELL('',(#15098,#15099,#15100,#15101,#15102,#15103));
#15574=CLOSED_SHELL('',(#15104,#15105,#15106,#15107,#15108,#15109,#15110,
#15111,#15112));
#15575=CLOSED_SHELL('',(#15113,#15114,#15115,#15116,#15117,#15118,#15119,
#15120,#15121));
#15576=CLOSED_SHELL('',(#15122,#15123,#15124,#15125,#15126,#15127,#15128,
#15129,#15130,#15131,#15132,#15133,#15134,#15135,#15136));
#15577=CLOSED_SHELL('',(#15137,#15138,#15139,#15140,#15141,#15142));
#15578=CLOSED_SHELL('',(#15143,#15144,#15145,#15146,#15147,#15148));
#15579=CLOSED_SHELL('',(#15149,#15150,#15151,#15152,#15153,#15154,#15155,
#15156));
#15580=CLOSED_SHELL('',(#15157,#15158,#15159,#15160,#15161,#15162,#15163,
#15164,#15165));
#15581=CLOSED_SHELL('',(#15166,#15167,#15168,#15169,#15170,#15171,#15172,
#15173,#15174));
#15582=CLOSED_SHELL('',(#15175,#15176,#15177,#15178,#15179,#15180,#15181,
#15182,#15183));
#15583=CLOSED_SHELL('',(#15184,#15185,#15186,#15187,#15188,#15189,#15190,
#15191,#15192));
#15584=CLOSED_SHELL('',(#15193,#15194,#15195,#15196,#15197,#15198));
#15585=CLOSED_SHELL('',(#15199,#15200,#15201,#15202,#15203,#15204));
#15586=CLOSED_SHELL('',(#15205,#15206,#15207,#15208,#15209,#15210));
#15587=CLOSED_SHELL('',(#15211,#15212,#15213,#15214,#15215,#15216));
#15588=CLOSED_SHELL('',(#15217,#15218,#15219,#15220,#15221,#15222));
#15589=CLOSED_SHELL('',(#15223,#15224,#15225,#15226,#15227,#15228,#15229,
#15230,#15231,#15232));
#15590=CLOSED_SHELL('',(#15233,#15234,#15235,#15236,#15237,#15238,#15239,
#15240,#15241,#15242,#15243,#15244));
#15591=CLOSED_SHELL('',(#15245,#15246,#15247,#15248,#15249,#15250,#15251,
#15252,#15253));
#15592=CLOSED_SHELL('',(#15254,#15255,#15256,#15257,#15258,#15259,#15260,
#15261,#15262));
#15593=CLOSED_SHELL('',(#15263,#15264,#15265,#15266,#15267,#15268,#15269,
#15270,#15271));
#15594=CLOSED_SHELL('',(#15272,#15273,#15274,#15275,#15276,#15277,#15278,
#15279,#15280));
#15595=CLOSED_SHELL('',(#15281,#15282,#15283,#15284,#15285,#15286,#15287,
#15288,#15289));
#15596=CLOSED_SHELL('',(#15290,#15291,#15292,#15293,#15294,#15295,#15296,
#15297,#15298));
#15597=CLOSED_SHELL('',(#15299,#15300,#15301,#15302,#15303,#15304,#15305,
#15306,#15307));
#15598=CLOSED_SHELL('',(#15308,#15309,#15310,#15311,#15312,#15313,#15314,
#15315,#15316));
#15599=CLOSED_SHELL('',(#15317,#15318,#15319,#15320,#15321,#15322,#15323,
#15324,#15325));
#15600=CLOSED_SHELL('',(#15326,#15327,#15328,#15329,#15330,#15331,#15332,
#15333,#15334));
#15601=CLOSED_SHELL('',(#15335,#15336,#15337,#15338,#15339,#15340,#15341,
#15342,#15343));
#15602=CLOSED_SHELL('',(#15344,#15345,#15346,#15347,#15348,#15349,#15350,
#15351,#15352,#15353));
#15603=CLOSED_SHELL('',(#15354,#15355,#15356,#15357,#15358,#15359));
#15604=CLOSED_SHELL('',(#15360,#15361,#15362,#15363,#15364,#15365));
#15605=CLOSED_SHELL('',(#15366,#15367,#15368,#15369,#15370,#15371));
#15606=CLOSED_SHELL('',(#15372,#15373,#15374,#15375,#15376,#15377));
#15607=CLOSED_SHELL('',(#15378,#15379,#15380,#15381,#15382,#15383));
#15608=CLOSED_SHELL('',(#15384,#15385,#15386,#15387,#15388,#15389));
#15609=CLOSED_SHELL('',(#15390,#15391,#15392,#15393,#15394,#15395));
#15610=CLOSED_SHELL('',(#15396,#15397,#15398,#15399,#15400,#15401));
#15611=CLOSED_SHELL('',(#15402,#15403,#15404,#15405,#15406,#15407));
#15612=CLOSED_SHELL('',(#15408,#15409,#15410,#15411,#15412,#15413));
#15613=CLOSED_SHELL('',(#15414,#15415,#15416,#15417,#15418,#15419));
#15614=CLOSED_SHELL('',(#15420,#15421,#15422,#15423,#15424,#15425));
#15615=CLOSED_SHELL('',(#15426,#15427,#15428,#15429,#15430,#15431));
#15616=CLOSED_SHELL('',(#15432,#15433,#15434,#15435,#15436,#15437));
#15617=CLOSED_SHELL('',(#15438,#15439,#15440,#15441,#15442,#15443));
#15618=CLOSED_SHELL('',(#15444,#15445,#15446,#15447,#15448,#15449));
#15619=CLOSED_SHELL('',(#15450,#15451,#15452,#15453,#15454,#15455));
#15620=CLOSED_SHELL('',(#15456,#15457,#15458,#15459,#15460,#15461));
#15621=CLOSED_SHELL('',(#15462,#15463,#15464,#15465,#15466,#15467));
#15622=CLOSED_SHELL('',(#15468,#15469,#15470,#15471,#15472,#15473));
#15623=CLOSED_SHELL('',(#15474,#15475,#15476,#15477,#15478,#15479));
#15624=CLOSED_SHELL('',(#15480,#15481,#15482,#15483,#15484,#15485));
#15625=CLOSED_SHELL('',(#15486,#15487,#15488,#15489,#15490,#15491,#15492,
#15493,#15494,#15495,#15496,#15497,#15498,#15499,#15500,#15501,#15502,#15503,
#15504,#15505,#15506,#15507,#15508,#15509,#15510));
#15626=CLOSED_SHELL('',(#15511,#15512,#15513,#15514));
#15627=CLOSED_SHELL('',(#15515,#15516,#15517,#15518,#15519,#15520,#15521,
#15522,#15523,#15524,#15525,#15526,#15527,#15528,#15529,#15530,#15531,#15532,
#15533,#15534,#15535,#15536,#15537,#15538));
#15628=DERIVED_UNIT_ELEMENT(#15656,1.);
#15629=DERIVED_UNIT_ELEMENT(#32905,-3.);
#15630=DERIVED_UNIT_ELEMENT(#15656,1.);
#15631=DERIVED_UNIT_ELEMENT(#32905,-3.);
#15632=DERIVED_UNIT_ELEMENT(#15656,1.);
#15633=DERIVED_UNIT_ELEMENT(#32905,-3.);
#15634=DERIVED_UNIT_ELEMENT(#15656,1.);
#15635=DERIVED_UNIT_ELEMENT(#32905,-3.);
#15636=DERIVED_UNIT_ELEMENT(#15656,1.);
#15637=DERIVED_UNIT_ELEMENT(#32905,-3.);
#15638=DERIVED_UNIT_ELEMENT(#15656,1.);
#15639=DERIVED_UNIT_ELEMENT(#32905,-3.);
#15640=DERIVED_UNIT_ELEMENT(#15656,1.);
#15641=DERIVED_UNIT_ELEMENT(#32905,-3.);
#15642=DERIVED_UNIT_ELEMENT(#15656,1.);
#15643=DERIVED_UNIT_ELEMENT(#32905,-3.);
#15644=DERIVED_UNIT_ELEMENT(#15656,1.);
#15645=DERIVED_UNIT_ELEMENT(#32905,-3.);
#15646=DERIVED_UNIT_ELEMENT(#15656,1.);
#15647=DERIVED_UNIT_ELEMENT(#32905,-3.);
#15648=DERIVED_UNIT_ELEMENT(#15656,1.);
#15649=DERIVED_UNIT_ELEMENT(#32905,-3.);
#15650=DERIVED_UNIT_ELEMENT(#15656,1.);
#15651=DERIVED_UNIT_ELEMENT(#32905,-3.);
#15652=DERIVED_UNIT_ELEMENT(#15656,1.);
#15653=DERIVED_UNIT_ELEMENT(#32905,-3.);
#15654=DERIVED_UNIT_ELEMENT(#15656,1.);
#15655=DERIVED_UNIT_ELEMENT(#32905,-3.);
#15656=(
MASS_UNIT()
NAMED_UNIT(*)
SI_UNIT(.KILO.,.GRAM.)
);
#15657=DERIVED_UNIT((#15628,#15629));
#15658=DERIVED_UNIT((#15630,#15631));
#15659=DERIVED_UNIT((#15632,#15633));
#15660=DERIVED_UNIT((#15634,#15635));
#15661=DERIVED_UNIT((#15636,#15637));
#15662=DERIVED_UNIT((#15638,#15639));
#15663=DERIVED_UNIT((#15640,#15641));
#15664=DERIVED_UNIT((#15642,#15643));
#15665=DERIVED_UNIT((#15644,#15645));
#15666=DERIVED_UNIT((#15646,#15647));
#15667=DERIVED_UNIT((#15648,#15649));
#15668=DERIVED_UNIT((#15650,#15651));
#15669=DERIVED_UNIT((#15652,#15653));
#15670=DERIVED_UNIT((#15654,#15655));
#15671=MEASURE_REPRESENTATION_ITEM('density measure',
POSITIVE_RATIO_MEASURE(7850.),#15657);
#15672=MEASURE_REPRESENTATION_ITEM('density measure',
POSITIVE_RATIO_MEASURE(7850.),#15658);
#15673=MEASURE_REPRESENTATION_ITEM('density measure',
POSITIVE_RATIO_MEASURE(7850.),#15659);
#15674=MEASURE_REPRESENTATION_ITEM('density measure',
POSITIVE_RATIO_MEASURE(7850.),#15660);
#15675=MEASURE_REPRESENTATION_ITEM('density measure',
POSITIVE_RATIO_MEASURE(7850.),#15661);
#15676=MEASURE_REPRESENTATION_ITEM('density measure',
POSITIVE_RATIO_MEASURE(7850.),#15662);
#15677=MEASURE_REPRESENTATION_ITEM('density measure',
POSITIVE_RATIO_MEASURE(7850.),#15663);
#15678=MEASURE_REPRESENTATION_ITEM('density measure',
POSITIVE_RATIO_MEASURE(7850.),#15664);
#15679=MEASURE_REPRESENTATION_ITEM('density measure',
POSITIVE_RATIO_MEASURE(7850.),#15665);
#15680=MEASURE_REPRESENTATION_ITEM('density measure',
POSITIVE_RATIO_MEASURE(7850.),#15666);
#15681=MEASURE_REPRESENTATION_ITEM('density measure',
POSITIVE_RATIO_MEASURE(7850.),#15667);
#15682=MEASURE_REPRESENTATION_ITEM('density measure',
POSITIVE_RATIO_MEASURE(7850.),#15668);
#15683=MEASURE_REPRESENTATION_ITEM('density measure',
POSITIVE_RATIO_MEASURE(7850.),#15669);
#15684=MEASURE_REPRESENTATION_ITEM('density measure',
POSITIVE_RATIO_MEASURE(7850.),#15670);
#15685=PROPERTY_DEFINITION_REPRESENTATION(#15755,#15713);
#15686=PROPERTY_DEFINITION_REPRESENTATION(#15756,#15714);
#15687=PROPERTY_DEFINITION_REPRESENTATION(#15757,#15715);
#15688=PROPERTY_DEFINITION_REPRESENTATION(#15758,#15716);
#15689=PROPERTY_DEFINITION_REPRESENTATION(#15759,#15717);
#15690=PROPERTY_DEFINITION_REPRESENTATION(#15760,#15718);
#15691=PROPERTY_DEFINITION_REPRESENTATION(#15761,#15719);
#15692=PROPERTY_DEFINITION_REPRESENTATION(#15762,#15720);
#15693=PROPERTY_DEFINITION_REPRESENTATION(#15763,#15721);
#15694=PROPERTY_DEFINITION_REPRESENTATION(#15764,#15722);
#15695=PROPERTY_DEFINITION_REPRESENTATION(#15765,#15723);
#15696=PROPERTY_DEFINITION_REPRESENTATION(#15766,#15724);
#15697=PROPERTY_DEFINITION_REPRESENTATION(#15767,#15725);
#15698=PROPERTY_DEFINITION_REPRESENTATION(#15768,#15726);
#15699=PROPERTY_DEFINITION_REPRESENTATION(#15769,#15727);
#15700=PROPERTY_DEFINITION_REPRESENTATION(#15770,#15728);
#15701=PROPERTY_DEFINITION_REPRESENTATION(#15771,#15729);
#15702=PROPERTY_DEFINITION_REPRESENTATION(#15772,#15730);
#15703=PROPERTY_DEFINITION_REPRESENTATION(#15773,#15731);
#15704=PROPERTY_DEFINITION_REPRESENTATION(#15774,#15732);
#15705=PROPERTY_DEFINITION_REPRESENTATION(#15775,#15733);
#15706=PROPERTY_DEFINITION_REPRESENTATION(#15776,#15734);
#15707=PROPERTY_DEFINITION_REPRESENTATION(#15777,#15735);
#15708=PROPERTY_DEFINITION_REPRESENTATION(#15778,#15736);
#15709=PROPERTY_DEFINITION_REPRESENTATION(#15779,#15737);
#15710=PROPERTY_DEFINITION_REPRESENTATION(#15780,#15738);
#15711=PROPERTY_DEFINITION_REPRESENTATION(#15781,#15739);
#15712=PROPERTY_DEFINITION_REPRESENTATION(#15782,#15740);
#15713=REPRESENTATION('material name',(#15741),#32888);
#15714=REPRESENTATION('density',(#15671),#32888);
#15715=REPRESENTATION('material name',(#15742),#32889);
#15716=REPRESENTATION('density',(#15672),#32889);
#15717=REPRESENTATION('material name',(#15743),#32891);
#15718=REPRESENTATION('density',(#15673),#32891);
#15719=REPRESENTATION('material name',(#15744),#32892);
#15720=REPRESENTATION('density',(#15674),#32892);
#15721=REPRESENTATION('material name',(#15745),#32893);
#15722=REPRESENTATION('density',(#15675),#32893);
#15723=REPRESENTATION('material name',(#15746),#32894);
#15724=REPRESENTATION('density',(#15676),#32894);
#15725=REPRESENTATION('material name',(#15747),#32895);
#15726=REPRESENTATION('density',(#15677),#32895);
#15727=REPRESENTATION('material name',(#15748),#32896);
#15728=REPRESENTATION('density',(#15678),#32896);
#15729=REPRESENTATION('material name',(#15749),#32897);
#15730=REPRESENTATION('density',(#15679),#32897);
#15731=REPRESENTATION('material name',(#15750),#32898);
#15732=REPRESENTATION('density',(#15680),#32898);
#15733=REPRESENTATION('material name',(#15751),#32899);
#15734=REPRESENTATION('density',(#15681),#32899);
#15735=REPRESENTATION('material name',(#15752),#32900);
#15736=REPRESENTATION('density',(#15682),#32900);
#15737=REPRESENTATION('material name',(#15753),#32901);
#15738=REPRESENTATION('density',(#15683),#32901);
#15739=REPRESENTATION('material name',(#15754),#32902);
#15740=REPRESENTATION('density',(#15684),#32902);
#15741=DESCRIPTIVE_REPRESENTATION_ITEM('Steel','Steel');
#15742=DESCRIPTIVE_REPRESENTATION_ITEM('Steel','Steel');
#15743=DESCRIPTIVE_REPRESENTATION_ITEM('Steel','Steel');
#15744=DESCRIPTIVE_REPRESENTATION_ITEM('Steel','Steel');
#15745=DESCRIPTIVE_REPRESENTATION_ITEM('Steel','Steel');
#15746=DESCRIPTIVE_REPRESENTATION_ITEM('Steel','Steel');
#15747=DESCRIPTIVE_REPRESENTATION_ITEM('Steel','Steel');
#15748=DESCRIPTIVE_REPRESENTATION_ITEM('Steel','Steel');
#15749=DESCRIPTIVE_REPRESENTATION_ITEM('Steel','Steel');
#15750=DESCRIPTIVE_REPRESENTATION_ITEM('Steel','Steel');
#15751=DESCRIPTIVE_REPRESENTATION_ITEM('Steel','Steel');
#15752=DESCRIPTIVE_REPRESENTATION_ITEM('Steel','Steel');
#15753=DESCRIPTIVE_REPRESENTATION_ITEM('Steel','Steel');
#15754=DESCRIPTIVE_REPRESENTATION_ITEM('Steel','Steel');
#15755=PROPERTY_DEFINITION('material property','material name',#33030);
#15756=PROPERTY_DEFINITION('material property','density of part',#33030);
#15757=PROPERTY_DEFINITION('material property','material name',#33031);
#15758=PROPERTY_DEFINITION('material property','density of part',#33031);
#15759=PROPERTY_DEFINITION('material property','material name',#33033);
#15760=PROPERTY_DEFINITION('material property','density of part',#33033);
#15761=PROPERTY_DEFINITION('material property','material name',#33034);
#15762=PROPERTY_DEFINITION('material property','density of part',#33034);
#15763=PROPERTY_DEFINITION('material property','material name',#33035);
#15764=PROPERTY_DEFINITION('material property','density of part',#33035);
#15765=PROPERTY_DEFINITION('material property','material name',#33036);
#15766=PROPERTY_DEFINITION('material property','density of part',#33036);
#15767=PROPERTY_DEFINITION('material property','material name',#33037);
#15768=PROPERTY_DEFINITION('material property','density of part',#33037);
#15769=PROPERTY_DEFINITION('material property','material name',#33038);
#15770=PROPERTY_DEFINITION('material property','density of part',#33038);
#15771=PROPERTY_DEFINITION('material property','material name',#33039);
#15772=PROPERTY_DEFINITION('material property','density of part',#33039);
#15773=PROPERTY_DEFINITION('material property','material name',#33040);
#15774=PROPERTY_DEFINITION('material property','density of part',#33040);
#15775=PROPERTY_DEFINITION('material property','material name',#33041);
#15776=PROPERTY_DEFINITION('material property','density of part',#33041);
#15777=PROPERTY_DEFINITION('material property','material name',#33042);
#15778=PROPERTY_DEFINITION('material property','density of part',#33042);
#15779=PROPERTY_DEFINITION('material property','material name',#33043);
#15780=PROPERTY_DEFINITION('material property','density of part',#33043);
#15781=PROPERTY_DEFINITION('material property','material name',#33044);
#15782=PROPERTY_DEFINITION('material property','density of part',#33044);
#15783=AXIS2_PLACEMENT_3D('',#21309,#17157,#17158);
#15784=AXIS2_PLACEMENT_3D('',#21310,#17159,#17160);
#15785=AXIS2_PLACEMENT_3D('',#21311,#17161,#17162);
#15786=AXIS2_PLACEMENT_3D('',#21320,#17167,#17168);
#15787=AXIS2_PLACEMENT_3D('',#21326,#17172,#17173);
#15788=AXIS2_PLACEMENT_3D('',#21332,#17177,#17178);
#15789=AXIS2_PLACEMENT_3D('',#21335,#17181,#17182);
#15790=AXIS2_PLACEMENT_3D('',#21344,#17187,#17188);
#15791=AXIS2_PLACEMENT_3D('',#21353,#17193,#17194);
#15792=AXIS2_PLACEMENT_3D('',#21356,#17197,#17198);
#15793=AXIS2_PLACEMENT_3D('',#21358,#17200,#17201);
#15794=AXIS2_PLACEMENT_3D('',#21360,#17203,#17204);
#15795=AXIS2_PLACEMENT_3D('',#21361,#17205,#17206);
#15796=AXIS2_PLACEMENT_3D('',#21370,#17211,#17212);
#15797=AXIS2_PLACEMENT_3D('',#21376,#17216,#17217);
#15798=AXIS2_PLACEMENT_3D('',#21378,#17218,#17219);
#15799=AXIS2_PLACEMENT_3D('',#21381,#17221,#17222);
#15800=AXIS2_PLACEMENT_3D('',#21382,#17223,#17224);
#15801=AXIS2_PLACEMENT_3D('',#21388,#17228,#17229);
#15802=AXIS2_PLACEMENT_3D('',#21394,#17233,#17234);
#15803=AXIS2_PLACEMENT_3D('',#21397,#17237,#17238);
#15804=AXIS2_PLACEMENT_3D('',#21398,#17239,#17240);
#15805=AXIS2_PLACEMENT_3D('',#21399,#17241,#17242);
#15806=AXIS2_PLACEMENT_3D('',#21408,#17247,#17248);
#15807=AXIS2_PLACEMENT_3D('',#21414,#17252,#17253);
#15808=AXIS2_PLACEMENT_3D('',#21416,#17254,#17255);
#15809=AXIS2_PLACEMENT_3D('',#21418,#17256,#17257);
#15810=AXIS2_PLACEMENT_3D('',#21420,#17259,#17260);
#15811=AXIS2_PLACEMENT_3D('',#21426,#17264,#17265);
#15812=AXIS2_PLACEMENT_3D('',#21432,#17269,#17270);
#15813=AXIS2_PLACEMENT_3D('',#21435,#17273,#17274);
#15814=AXIS2_PLACEMENT_3D('',#21436,#17275,#17276);
#15815=AXIS2_PLACEMENT_3D('',#21437,#17277,#17278);
#15816=AXIS2_PLACEMENT_3D('',#21439,#17279,#17280);
#15817=AXIS2_PLACEMENT_3D('',#21442,#17282,#17283);
#15818=AXIS2_PLACEMENT_3D('',#21443,#17284,#17285);
#15819=AXIS2_PLACEMENT_3D('',#21445,#17286,#17287);
#15820=AXIS2_PLACEMENT_3D('',#21448,#17289,#17290);
#15821=AXIS2_PLACEMENT_3D('',#21449,#17291,#17292);
#15822=AXIS2_PLACEMENT_3D('',#21451,#17293,#17294);
#15823=AXIS2_PLACEMENT_3D('',#21454,#17296,#17297);
#15824=AXIS2_PLACEMENT_3D('',#21455,#17298,#17299);
#15825=AXIS2_PLACEMENT_3D('',#21457,#17300,#17301);
#15826=AXIS2_PLACEMENT_3D('',#21460,#17303,#17304);
#15827=AXIS2_PLACEMENT_3D('',#21461,#17305,#17306);
#15828=AXIS2_PLACEMENT_3D('',#21463,#17307,#17308);
#15829=AXIS2_PLACEMENT_3D('',#21466,#17310,#17311);
#15830=AXIS2_PLACEMENT_3D('',#21467,#17312,#17313);
#15831=AXIS2_PLACEMENT_3D('',#21469,#17314,#17315);
#15832=AXIS2_PLACEMENT_3D('',#21472,#17317,#17318);
#15833=AXIS2_PLACEMENT_3D('',#21473,#17319,#17320);
#15834=AXIS2_PLACEMENT_3D('',#21482,#17325,#17326);
#15835=AXIS2_PLACEMENT_3D('',#21491,#17331,#17332);
#15836=AXIS2_PLACEMENT_3D('',#21494,#17335,#17336);
#15837=AXIS2_PLACEMENT_3D('',#21496,#17338,#17339);
#15838=AXIS2_PLACEMENT_3D('',#21498,#17341,#17342);
#15839=AXIS2_PLACEMENT_3D('',#21499,#17343,#17344);
#15840=AXIS2_PLACEMENT_3D('',#21501,#17345,#17346);
#15841=AXIS2_PLACEMENT_3D('',#21504,#17348,#17349);
#15842=AXIS2_PLACEMENT_3D('',#21505,#17350,#17351);
#15843=AXIS2_PLACEMENT_3D('',#21507,#17352,#17353);
#15844=AXIS2_PLACEMENT_3D('',#21510,#17355,#17356);
#15845=AXIS2_PLACEMENT_3D('',#21511,#17357,#17358);
#15846=AXIS2_PLACEMENT_3D('',#21513,#17359,#17360);
#15847=AXIS2_PLACEMENT_3D('',#21516,#17362,#17363);
#15848=AXIS2_PLACEMENT_3D('',#21517,#17364,#17365);
#15849=AXIS2_PLACEMENT_3D('',#21519,#17366,#17367);
#15850=AXIS2_PLACEMENT_3D('',#21522,#17369,#17370);
#15851=AXIS2_PLACEMENT_3D('',#21523,#17371,#17372);
#15852=AXIS2_PLACEMENT_3D('',#21525,#17373,#17374);
#15853=AXIS2_PLACEMENT_3D('',#21528,#17376,#17377);
#15854=AXIS2_PLACEMENT_3D('',#21529,#17378,#17379);
#15855=AXIS2_PLACEMENT_3D('',#21538,#17384,#17385);
#15856=AXIS2_PLACEMENT_3D('',#21544,#17389,#17390);
#15857=AXIS2_PLACEMENT_3D('',#21550,#17394,#17395);
#15858=AXIS2_PLACEMENT_3D('',#21553,#17398,#17399);
#15859=AXIS2_PLACEMENT_3D('',#21554,#17400,#17401);
#15860=AXIS2_PLACEMENT_3D('',#21555,#17402,#17403);
#15861=AXIS2_PLACEMENT_3D('',#21557,#17404,#17405);
#15862=AXIS2_PLACEMENT_3D('',#21560,#17407,#17408);
#15863=AXIS2_PLACEMENT_3D('',#21561,#17409,#17410);
#15864=AXIS2_PLACEMENT_3D('',#21563,#17411,#17412);
#15865=AXIS2_PLACEMENT_3D('',#21566,#17414,#17415);
#15866=AXIS2_PLACEMENT_3D('',#21567,#17416,#17417);
#15867=AXIS2_PLACEMENT_3D('',#21569,#17418,#17419);
#15868=AXIS2_PLACEMENT_3D('',#21572,#17421,#17422);
#15869=AXIS2_PLACEMENT_3D('',#21573,#17423,#17424);
#15870=AXIS2_PLACEMENT_3D('',#21575,#17425,#17426);
#15871=AXIS2_PLACEMENT_3D('',#21578,#17428,#17429);
#15872=AXIS2_PLACEMENT_3D('',#21579,#17430,#17431);
#15873=AXIS2_PLACEMENT_3D('',#21581,#17432,#17433);
#15874=AXIS2_PLACEMENT_3D('',#21584,#17435,#17436);
#15875=AXIS2_PLACEMENT_3D('',#21585,#17437,#17438);
#15876=AXIS2_PLACEMENT_3D('',#21594,#17443,#17444);
#15877=AXIS2_PLACEMENT_3D('',#21600,#17448,#17449);
#15878=AXIS2_PLACEMENT_3D('',#21606,#17453,#17454);
#15879=AXIS2_PLACEMENT_3D('',#21609,#17457,#17458);
#15880=AXIS2_PLACEMENT_3D('',#21610,#17459,#17460);
#15881=AXIS2_PLACEMENT_3D('',#21611,#17461,#17462);
#15882=AXIS2_PLACEMENT_3D('',#21620,#17467,#17468);
#15883=AXIS2_PLACEMENT_3D('',#21626,#17472,#17473);
#15884=AXIS2_PLACEMENT_3D('',#21632,#17477,#17478);
#15885=AXIS2_PLACEMENT_3D('',#21635,#17481,#17482);
#15886=AXIS2_PLACEMENT_3D('',#21636,#17483,#17484);
#15887=AXIS2_PLACEMENT_3D('',#21637,#17485,#17486);
#15888=AXIS2_PLACEMENT_3D('',#21646,#17491,#17492);
#15889=AXIS2_PLACEMENT_3D('',#21652,#17496,#17497);
#15890=AXIS2_PLACEMENT_3D('',#21658,#17501,#17502);
#15891=AXIS2_PLACEMENT_3D('',#21661,#17505,#17506);
#15892=AXIS2_PLACEMENT_3D('',#21662,#17507,#17508);
#15893=AXIS2_PLACEMENT_3D('',#21663,#17509,#17510);
#15894=AXIS2_PLACEMENT_3D('',#21672,#17515,#17516);
#15895=AXIS2_PLACEMENT_3D('',#21678,#17520,#17521);
#15896=AXIS2_PLACEMENT_3D('',#21684,#17525,#17526);
#15897=AXIS2_PLACEMENT_3D('',#21687,#17529,#17530);
#15898=AXIS2_PLACEMENT_3D('',#21688,#17531,#17532);
#15899=AXIS2_PLACEMENT_3D('',#21689,#17533,#17534);
#15900=AXIS2_PLACEMENT_3D('',#21690,#17535,#17536);
#15901=AXIS2_PLACEMENT_3D('',#21692,#17537,#17538);
#15902=AXIS2_PLACEMENT_3D('',#21695,#17540,#17541);
#15903=AXIS2_PLACEMENT_3D('',#21696,#17542,#17543);
#15904=AXIS2_PLACEMENT_3D('',#21698,#17544,#17545);
#15905=AXIS2_PLACEMENT_3D('',#21701,#17547,#17548);
#15906=AXIS2_PLACEMENT_3D('',#21702,#17549,#17550);
#15907=AXIS2_PLACEMENT_3D('',#21704,#17551,#17552);
#15908=AXIS2_PLACEMENT_3D('',#21707,#17554,#17555);
#15909=AXIS2_PLACEMENT_3D('',#21708,#17556,#17557);
#15910=AXIS2_PLACEMENT_3D('',#21710,#17558,#17559);
#15911=AXIS2_PLACEMENT_3D('',#21713,#17561,#17562);
#15912=AXIS2_PLACEMENT_3D('',#21714,#17563,#17564);
#15913=AXIS2_PLACEMENT_3D('',#21716,#17565,#17566);
#15914=AXIS2_PLACEMENT_3D('',#21719,#17568,#17569);
#15915=AXIS2_PLACEMENT_3D('',#21720,#17570,#17571);
#15916=AXIS2_PLACEMENT_3D('',#21722,#17572,#17573);
#15917=AXIS2_PLACEMENT_3D('',#21725,#17575,#17576);
#15918=AXIS2_PLACEMENT_3D('',#21726,#17577,#17578);
#15919=AXIS2_PLACEMENT_3D('',#21728,#17579,#17580);
#15920=AXIS2_PLACEMENT_3D('',#21731,#17582,#17583);
#15921=AXIS2_PLACEMENT_3D('',#21732,#17584,#17585);
#15922=AXIS2_PLACEMENT_3D('',#21734,#17586,#17587);
#15923=AXIS2_PLACEMENT_3D('',#21737,#17589,#17590);
#15924=AXIS2_PLACEMENT_3D('',#21738,#17591,#17592);
#15925=AXIS2_PLACEMENT_3D('',#21740,#17593,#17594);
#15926=AXIS2_PLACEMENT_3D('',#21743,#17596,#17597);
#15927=AXIS2_PLACEMENT_3D('',#21744,#17598,#17599);
#15928=AXIS2_PLACEMENT_3D('',#21746,#17600,#17601);
#15929=AXIS2_PLACEMENT_3D('',#21749,#17603,#17604);
#15930=AXIS2_PLACEMENT_3D('',#21750,#17605,#17606);
#15931=AXIS2_PLACEMENT_3D('',#21752,#17607,#17608);
#15932=AXIS2_PLACEMENT_3D('',#21755,#17610,#17611);
#15933=AXIS2_PLACEMENT_3D('',#21756,#17612,#17613);
#15934=AXIS2_PLACEMENT_3D('',#21758,#17614,#17615);
#15935=AXIS2_PLACEMENT_3D('',#21761,#17617,#17618);
#15936=AXIS2_PLACEMENT_3D('',#21762,#17619,#17620);
#15937=AXIS2_PLACEMENT_3D('',#21764,#17621,#17622);
#15938=AXIS2_PLACEMENT_3D('',#21767,#17624,#17625);
#15939=AXIS2_PLACEMENT_3D('',#21768,#17626,#17627);
#15940=AXIS2_PLACEMENT_3D('',#21770,#17628,#17629);
#15941=AXIS2_PLACEMENT_3D('',#21773,#17631,#17632);
#15942=AXIS2_PLACEMENT_3D('',#21774,#17633,#17634);
#15943=AXIS2_PLACEMENT_3D('',#21776,#17635,#17636);
#15944=AXIS2_PLACEMENT_3D('',#21779,#17638,#17639);
#15945=AXIS2_PLACEMENT_3D('',#21780,#17640,#17641);
#15946=AXIS2_PLACEMENT_3D('',#21782,#17642,#17643);
#15947=AXIS2_PLACEMENT_3D('',#21785,#17645,#17646);
#15948=AXIS2_PLACEMENT_3D('',#21786,#17647,#17648);
#15949=AXIS2_PLACEMENT_3D('',#21788,#17649,#17650);
#15950=AXIS2_PLACEMENT_3D('',#21791,#17652,#17653);
#15951=AXIS2_PLACEMENT_3D('',#21792,#17654,#17655);
#15952=AXIS2_PLACEMENT_3D('',#21794,#17656,#17657);
#15953=AXIS2_PLACEMENT_3D('',#21797,#17659,#17660);
#15954=AXIS2_PLACEMENT_3D('',#21798,#17661,#17662);
#15955=AXIS2_PLACEMENT_3D('',#21807,#17667,#17668);
#15956=AXIS2_PLACEMENT_3D('',#21813,#17672,#17673);
#15957=AXIS2_PLACEMENT_3D('',#21819,#17677,#17678);
#15958=AXIS2_PLACEMENT_3D('',#21822,#17681,#17682);
#15959=AXIS2_PLACEMENT_3D('',#21823,#17683,#17684);
#15960=AXIS2_PLACEMENT_3D('',#21824,#17685,#17686);
#15961=AXIS2_PLACEMENT_3D('',#21826,#17687,#17688);
#15962=AXIS2_PLACEMENT_3D('',#21829,#17690,#17691);
#15963=AXIS2_PLACEMENT_3D('',#21830,#17692,#17693);
#15964=AXIS2_PLACEMENT_3D('',#21832,#17694,#17695);
#15965=AXIS2_PLACEMENT_3D('',#21835,#17697,#17698);
#15966=AXIS2_PLACEMENT_3D('',#21836,#17699,#17700);
#15967=AXIS2_PLACEMENT_3D('',#21837,#17701,#17702);
#15968=AXIS2_PLACEMENT_3D('',#21838,#17703,#17704);
#15969=AXIS2_PLACEMENT_3D('',#21840,#17705,#17706);
#15970=AXIS2_PLACEMENT_3D('',#21843,#17708,#17709);
#15971=AXIS2_PLACEMENT_3D('',#21844,#17710,#17711);
#15972=AXIS2_PLACEMENT_3D('',#21846,#17712,#17713);
#15973=AXIS2_PLACEMENT_3D('',#21849,#17715,#17716);
#15974=AXIS2_PLACEMENT_3D('',#21850,#17717,#17718);
#15975=AXIS2_PLACEMENT_3D('',#21851,#17719,#17720);
#15976=AXIS2_PLACEMENT_3D('',#21852,#17721,#17722);
#15977=AXIS2_PLACEMENT_3D('',#21854,#17723,#17724);
#15978=AXIS2_PLACEMENT_3D('',#21857,#17726,#17727);
#15979=AXIS2_PLACEMENT_3D('',#21858,#17728,#17729);
#15980=AXIS2_PLACEMENT_3D('',#21860,#17730,#17731);
#15981=AXIS2_PLACEMENT_3D('',#21863,#17733,#17734);
#15982=AXIS2_PLACEMENT_3D('',#21864,#17735,#17736);
#15983=AXIS2_PLACEMENT_3D('',#21866,#17737,#17738);
#15984=AXIS2_PLACEMENT_3D('',#21869,#17740,#17741);
#15985=AXIS2_PLACEMENT_3D('',#21870,#17742,#17743);
#15986=AXIS2_PLACEMENT_3D('',#21872,#17744,#17745);
#15987=AXIS2_PLACEMENT_3D('',#21875,#17747,#17748);
#15988=AXIS2_PLACEMENT_3D('',#21876,#17749,#17750);
#15989=AXIS2_PLACEMENT_3D('',#21878,#17751,#17752);
#15990=AXIS2_PLACEMENT_3D('',#21881,#17754,#17755);
#15991=AXIS2_PLACEMENT_3D('',#21882,#17756,#17757);
#15992=AXIS2_PLACEMENT_3D('',#21884,#17758,#17759);
#15993=AXIS2_PLACEMENT_3D('',#21887,#17761,#17762);
#15994=AXIS2_PLACEMENT_3D('',#21888,#17763,#17764);
#15995=AXIS2_PLACEMENT_3D('',#21890,#17765,#17766);
#15996=AXIS2_PLACEMENT_3D('',#21893,#17768,#17769);
#15997=AXIS2_PLACEMENT_3D('',#21894,#17770,#17771);
#15998=AXIS2_PLACEMENT_3D('',#21896,#17772,#17773);
#15999=AXIS2_PLACEMENT_3D('',#21899,#17775,#17776);
#16000=AXIS2_PLACEMENT_3D('',#21900,#17777,#17778);
#16001=AXIS2_PLACEMENT_3D('',#21902,#17779,#17780);
#16002=AXIS2_PLACEMENT_3D('',#21905,#17782,#17783);
#16003=AXIS2_PLACEMENT_3D('',#21906,#17784,#17785);
#16004=AXIS2_PLACEMENT_3D('',#21908,#17786,#17787);
#16005=AXIS2_PLACEMENT_3D('',#21911,#17789,#17790);
#16006=AXIS2_PLACEMENT_3D('',#21912,#17791,#17792);
#16007=AXIS2_PLACEMENT_3D('',#21914,#17793,#17794);
#16008=AXIS2_PLACEMENT_3D('',#21917,#17796,#17797);
#16009=AXIS2_PLACEMENT_3D('',#21918,#17798,#17799);
#16010=AXIS2_PLACEMENT_3D('',#21920,#17800,#17801);
#16011=AXIS2_PLACEMENT_3D('',#21923,#17803,#17804);
#16012=AXIS2_PLACEMENT_3D('',#21924,#17805,#17806);
#16013=AXIS2_PLACEMENT_3D('',#21926,#17807,#17808);
#16014=AXIS2_PLACEMENT_3D('',#21929,#17810,#17811);
#16015=AXIS2_PLACEMENT_3D('',#21930,#17812,#17813);
#16016=AXIS2_PLACEMENT_3D('',#21932,#17814,#17815);
#16017=AXIS2_PLACEMENT_3D('',#21935,#17817,#17818);
#16018=AXIS2_PLACEMENT_3D('',#21936,#17819,#17820);
#16019=AXIS2_PLACEMENT_3D('',#21937,#17821,#17822);
#16020=AXIS2_PLACEMENT_3D('',#21938,#17823,#17824);
#16021=AXIS2_PLACEMENT_3D('',#21940,#17825,#17826);
#16022=AXIS2_PLACEMENT_3D('',#21943,#17828,#17829);
#16023=AXIS2_PLACEMENT_3D('',#21944,#17830,#17831);
#16024=AXIS2_PLACEMENT_3D('',#21946,#17832,#17833);
#16025=AXIS2_PLACEMENT_3D('',#21949,#17835,#17836);
#16026=AXIS2_PLACEMENT_3D('',#21950,#17837,#17838);
#16027=AXIS2_PLACEMENT_3D('',#21952,#17839,#17840);
#16028=AXIS2_PLACEMENT_3D('',#21955,#17842,#17843);
#16029=AXIS2_PLACEMENT_3D('',#21956,#17844,#17845);
#16030=AXIS2_PLACEMENT_3D('',#21958,#17846,#17847);
#16031=AXIS2_PLACEMENT_3D('',#21961,#17849,#17850);
#16032=AXIS2_PLACEMENT_3D('',#21962,#17851,#17852);
#16033=AXIS2_PLACEMENT_3D('',#21964,#17853,#17854);
#16034=AXIS2_PLACEMENT_3D('',#21967,#17856,#17857);
#16035=AXIS2_PLACEMENT_3D('',#21968,#17858,#17859);
#16036=AXIS2_PLACEMENT_3D('',#21970,#17860,#17861);
#16037=AXIS2_PLACEMENT_3D('',#21973,#17863,#17864);
#16038=AXIS2_PLACEMENT_3D('',#21974,#17865,#17866);
#16039=AXIS2_PLACEMENT_3D('',#21975,#17867,#17868);
#16040=AXIS2_PLACEMENT_3D('',#21976,#17869,#17870);
#16041=AXIS2_PLACEMENT_3D('',#21977,#17871,#17872);
#16042=AXIS2_PLACEMENT_3D('',#21978,#17873,#17874);
#16043=AXIS2_PLACEMENT_3D('',#21989,#17879,#17880);
#16044=AXIS2_PLACEMENT_3D('',#21993,#17882,#17883);
#16045=AXIS2_PLACEMENT_3D('',#21996,#17885,#17886);
#16046=AXIS2_PLACEMENT_3D('',#21997,#17887,#17888);
#16047=AXIS2_PLACEMENT_3D('',#22004,#17891,#17892);
#16048=AXIS2_PLACEMENT_3D('',#22008,#17894,#17895);
#16049=AXIS2_PLACEMENT_3D('',#22012,#17897,#17898);
#16050=AXIS2_PLACEMENT_3D('',#22016,#17901,#17902);
#16051=AXIS2_PLACEMENT_3D('',#22019,#17905,#17906);
#16052=AXIS2_PLACEMENT_3D('',#22021,#17908,#17909);
#16053=AXIS2_PLACEMENT_3D('',#22023,#17911,#17912);
#16054=AXIS2_PLACEMENT_3D('',#22025,#17914,#17915);
#16055=AXIS2_PLACEMENT_3D('',#22027,#17917,#17918);
#16056=AXIS2_PLACEMENT_3D('',#22029,#17920,#17921);
#16057=AXIS2_PLACEMENT_3D('',#22031,#17923,#17924);
#16058=AXIS2_PLACEMENT_3D('',#22033,#17926,#17927);
#16059=AXIS2_PLACEMENT_3D('',#22034,#17928,#17929);
#16060=AXIS2_PLACEMENT_3D('',#22039,#17931,#17932);
#16061=AXIS2_PLACEMENT_3D('',#22043,#17934,#17935);
#16062=AXIS2_PLACEMENT_3D('',#22047,#17937,#17938);
#16063=AXIS2_PLACEMENT_3D('',#22053,#17942,#17943);
#16064=AXIS2_PLACEMENT_3D('',#22062,#17947,#17948);
#16065=AXIS2_PLACEMENT_3D('',#22066,#17950,#17951);
#16066=AXIS2_PLACEMENT_3D('',#22070,#17953,#17954);
#16067=AXIS2_PLACEMENT_3D('',#22072,#17956,#17957);
#16068=AXIS2_PLACEMENT_3D('',#22075,#17960,#17961);
#16069=AXIS2_PLACEMENT_3D('',#22077,#17963,#17964);
#16070=AXIS2_PLACEMENT_3D('',#22079,#17966,#17967);
#16071=AXIS2_PLACEMENT_3D('',#22081,#17969,#17970);
#16072=AXIS2_PLACEMENT_3D('',#22083,#17972,#17973);
#16073=AXIS2_PLACEMENT_3D('',#22085,#17975,#17976);
#16074=AXIS2_PLACEMENT_3D('',#22087,#17978,#17979);
#16075=AXIS2_PLACEMENT_3D('',#22089,#17981,#17982);
#16076=AXIS2_PLACEMENT_3D('',#22090,#17983,#17984);
#16077=AXIS2_PLACEMENT_3D('',#22095,#17986,#17987);
#16078=AXIS2_PLACEMENT_3D('',#22099,#17989,#17990);
#16079=AXIS2_PLACEMENT_3D('',#22103,#17992,#17993);
#16080=AXIS2_PLACEMENT_3D('',#22109,#17997,#17998);
#16081=AXIS2_PLACEMENT_3D('',#22118,#18002,#18003);
#16082=AXIS2_PLACEMENT_3D('',#22122,#18005,#18006);
#16083=AXIS2_PLACEMENT_3D('',#22126,#18008,#18009);
#16084=AXIS2_PLACEMENT_3D('',#22128,#18011,#18012);
#16085=AXIS2_PLACEMENT_3D('',#22131,#18015,#18016);
#16086=AXIS2_PLACEMENT_3D('',#22133,#18018,#18019);
#16087=AXIS2_PLACEMENT_3D('',#22135,#18021,#18022);
#16088=AXIS2_PLACEMENT_3D('',#22137,#18024,#18025);
#16089=AXIS2_PLACEMENT_3D('',#22139,#18027,#18028);
#16090=AXIS2_PLACEMENT_3D('',#22141,#18030,#18031);
#16091=AXIS2_PLACEMENT_3D('',#22143,#18033,#18034);
#16092=AXIS2_PLACEMENT_3D('',#22145,#18036,#18037);
#16093=AXIS2_PLACEMENT_3D('',#22146,#18038,#18039);
#16094=AXIS2_PLACEMENT_3D('',#22148,#18040,#18041);
#16095=AXIS2_PLACEMENT_3D('',#22151,#18043,#18044);
#16096=AXIS2_PLACEMENT_3D('',#22152,#18045,#18046);
#16097=AXIS2_PLACEMENT_3D('',#22155,#18047,#18048);
#16098=AXIS2_PLACEMENT_3D('',#22159,#18050,#18051);
#16099=AXIS2_PLACEMENT_3D('',#22161,#18053,#18054);
#16100=AXIS2_PLACEMENT_3D('',#22163,#18055,#18056);
#16101=AXIS2_PLACEMENT_3D('',#22166,#18058,#18059);
#16102=AXIS2_PLACEMENT_3D('',#22167,#18060,#18061);
#16103=AXIS2_PLACEMENT_3D('',#22173,#18065,#18066);
#16104=AXIS2_PLACEMENT_3D('',#22179,#18070,#18071);
#16105=AXIS2_PLACEMENT_3D('',#22185,#18075,#18076);
#16106=AXIS2_PLACEMENT_3D('',#22188,#18079,#18080);
#16107=AXIS2_PLACEMENT_3D('',#22189,#18081,#18082);
#16108=AXIS2_PLACEMENT_3D('',#22190,#18083,#18084);
#16109=AXIS2_PLACEMENT_3D('',#22192,#18085,#18086);
#16110=AXIS2_PLACEMENT_3D('',#22195,#18088,#18089);
#16111=AXIS2_PLACEMENT_3D('',#22196,#18090,#18091);
#16112=AXIS2_PLACEMENT_3D('',#22205,#18095,#18096);
#16113=AXIS2_PLACEMENT_3D('',#22209,#18099,#18100);
#16114=AXIS2_PLACEMENT_3D('',#22218,#18104,#18105);
#16115=AXIS2_PLACEMENT_3D('',#22222,#18108,#18109);
#16116=AXIS2_PLACEMENT_3D('',#22225,#18112,#18113);
#16117=AXIS2_PLACEMENT_3D('',#22227,#18115,#18116);
#16118=AXIS2_PLACEMENT_3D('',#22229,#18118,#18119);
#16119=AXIS2_PLACEMENT_3D('',#22231,#18121,#18122);
#16120=AXIS2_PLACEMENT_3D('',#22233,#18124,#18125);
#16121=AXIS2_PLACEMENT_3D('',#22234,#18126,#18127);
#16122=AXIS2_PLACEMENT_3D('',#22236,#18128,#18129);
#16123=AXIS2_PLACEMENT_3D('',#22239,#18131,#18132);
#16124=AXIS2_PLACEMENT_3D('',#22240,#18133,#18134);
#16125=AXIS2_PLACEMENT_3D('',#22243,#18135,#18136);
#16126=AXIS2_PLACEMENT_3D('',#22247,#18138,#18139);
#16127=AXIS2_PLACEMENT_3D('',#22249,#18141,#18142);
#16128=AXIS2_PLACEMENT_3D('',#22251,#18143,#18144);
#16129=AXIS2_PLACEMENT_3D('',#22253,#18145,#18146);
#16130=AXIS2_PLACEMENT_3D('',#22255,#18148,#18149);
#16131=AXIS2_PLACEMENT_3D('',#22261,#18153,#18154);
#16132=AXIS2_PLACEMENT_3D('',#22267,#18158,#18159);
#16133=AXIS2_PLACEMENT_3D('',#22273,#18163,#18164);
#16134=AXIS2_PLACEMENT_3D('',#22276,#18167,#18168);
#16135=AXIS2_PLACEMENT_3D('',#22277,#18169,#18170);
#16136=AXIS2_PLACEMENT_3D('',#22278,#18171,#18172);
#16137=AXIS2_PLACEMENT_3D('',#22280,#18173,#18174);
#16138=AXIS2_PLACEMENT_3D('',#22283,#18176,#18177);
#16139=AXIS2_PLACEMENT_3D('',#22284,#18178,#18179);
#16140=AXIS2_PLACEMENT_3D('',#22293,#18183,#18184);
#16141=AXIS2_PLACEMENT_3D('',#22297,#18187,#18188);
#16142=AXIS2_PLACEMENT_3D('',#22306,#18192,#18193);
#16143=AXIS2_PLACEMENT_3D('',#22310,#18196,#18197);
#16144=AXIS2_PLACEMENT_3D('',#22313,#18200,#18201);
#16145=AXIS2_PLACEMENT_3D('',#22315,#18203,#18204);
#16146=AXIS2_PLACEMENT_3D('',#22317,#18206,#18207);
#16147=AXIS2_PLACEMENT_3D('',#22319,#18209,#18210);
#16148=AXIS2_PLACEMENT_3D('',#22321,#18212,#18213);
#16149=AXIS2_PLACEMENT_3D('',#22322,#18214,#18215);
#16150=AXIS2_PLACEMENT_3D('',#22325,#18216,#18217);
#16151=AXIS2_PLACEMENT_3D('',#22329,#18219,#18220);
#16152=AXIS2_PLACEMENT_3D('',#22331,#18222,#18223);
#16153=AXIS2_PLACEMENT_3D('',#22334,#18224,#18225);
#16154=AXIS2_PLACEMENT_3D('',#22338,#18227,#18228);
#16155=AXIS2_PLACEMENT_3D('',#22340,#18230,#18231);
#16156=AXIS2_PLACEMENT_3D('',#22343,#18232,#18233);
#16157=AXIS2_PLACEMENT_3D('',#22347,#18235,#18236);
#16158=AXIS2_PLACEMENT_3D('',#22349,#18238,#18239);
#16159=AXIS2_PLACEMENT_3D('',#22352,#18240,#18241);
#16160=AXIS2_PLACEMENT_3D('',#22356,#18243,#18244);
#16161=AXIS2_PLACEMENT_3D('',#22358,#18246,#18247);
#16162=AXIS2_PLACEMENT_3D('',#22364,#18251,#18252);
#16163=AXIS2_PLACEMENT_3D('',#22370,#18256,#18257);
#16164=AXIS2_PLACEMENT_3D('',#22375,#18259,#18260);
#16165=AXIS2_PLACEMENT_3D('',#22379,#18262,#18263);
#16166=AXIS2_PLACEMENT_3D('',#22383,#18265,#18266);
#16167=AXIS2_PLACEMENT_3D('',#22389,#18270,#18271);
#16168=AXIS2_PLACEMENT_3D('',#22397,#18275,#18276);
#16169=AXIS2_PLACEMENT_3D('',#22401,#18278,#18279);
#16170=AXIS2_PLACEMENT_3D('',#22403,#18281,#18282);
#16171=AXIS2_PLACEMENT_3D('',#22411,#18289,#18290);
#16172=AXIS2_PLACEMENT_3D('',#22413,#18292,#18293);
#16173=AXIS2_PLACEMENT_3D('',#22415,#18295,#18296);
#16174=AXIS2_PLACEMENT_3D('',#22417,#18298,#18299);
#16175=AXIS2_PLACEMENT_3D('',#22419,#18301,#18302);
#16176=AXIS2_PLACEMENT_3D('',#22421,#18304,#18305);
#16177=AXIS2_PLACEMENT_3D('',#22428,#18311,#18312);
#16178=AXIS2_PLACEMENT_3D('',#22430,#18313,#18314);
#16179=AXIS2_PLACEMENT_3D('',#22432,#18316,#18317);
#16180=AXIS2_PLACEMENT_3D('',#22434,#18319,#18320);
#16181=AXIS2_PLACEMENT_3D('',#22435,#18321,#18322);
#16182=AXIS2_PLACEMENT_3D('',#22436,#18323,#18324);
#16183=AXIS2_PLACEMENT_3D('',#22437,#18325,#18326);
#16184=AXIS2_PLACEMENT_3D('',#22438,#18327,#18328);
#16185=AXIS2_PLACEMENT_3D('',#22440,#18329,#18330);
#16186=AXIS2_PLACEMENT_3D('',#22443,#18332,#18333);
#16187=AXIS2_PLACEMENT_3D('',#22444,#18334,#18335);
#16188=AXIS2_PLACEMENT_3D('',#22453,#18339,#18340);
#16189=AXIS2_PLACEMENT_3D('',#22457,#18343,#18344);
#16190=AXIS2_PLACEMENT_3D('',#22466,#18348,#18349);
#16191=AXIS2_PLACEMENT_3D('',#22470,#18352,#18353);
#16192=AXIS2_PLACEMENT_3D('',#22473,#18356,#18357);
#16193=AXIS2_PLACEMENT_3D('',#22475,#18359,#18360);
#16194=AXIS2_PLACEMENT_3D('',#22477,#18362,#18363);
#16195=AXIS2_PLACEMENT_3D('',#22479,#18365,#18366);
#16196=AXIS2_PLACEMENT_3D('',#22481,#18368,#18369);
#16197=AXIS2_PLACEMENT_3D('',#22482,#18370,#18371);
#16198=AXIS2_PLACEMENT_3D('',#22484,#18372,#18373);
#16199=AXIS2_PLACEMENT_3D('',#22487,#18375,#18376);
#16200=AXIS2_PLACEMENT_3D('',#22488,#18377,#18378);
#16201=AXIS2_PLACEMENT_3D('',#22497,#18382,#18383);
#16202=AXIS2_PLACEMENT_3D('',#22501,#18386,#18387);
#16203=AXIS2_PLACEMENT_3D('',#22510,#18391,#18392);
#16204=AXIS2_PLACEMENT_3D('',#22514,#18395,#18396);
#16205=AXIS2_PLACEMENT_3D('',#22517,#18399,#18400);
#16206=AXIS2_PLACEMENT_3D('',#22519,#18402,#18403);
#16207=AXIS2_PLACEMENT_3D('',#22521,#18405,#18406);
#16208=AXIS2_PLACEMENT_3D('',#22523,#18408,#18409);
#16209=AXIS2_PLACEMENT_3D('',#22525,#18411,#18412);
#16210=AXIS2_PLACEMENT_3D('',#22526,#18413,#18414);
#16211=AXIS2_PLACEMENT_3D('',#22527,#18415,#18416);
#16212=AXIS2_PLACEMENT_3D('',#22536,#18421,#18422);
#16213=AXIS2_PLACEMENT_3D('',#22542,#18426,#18427);
#16214=AXIS2_PLACEMENT_3D('',#22544,#18428,#18429);
#16215=AXIS2_PLACEMENT_3D('',#22547,#18431,#18432);
#16216=AXIS2_PLACEMENT_3D('',#22548,#18433,#18434);
#16217=AXIS2_PLACEMENT_3D('',#22554,#18438,#18439);
#16218=AXIS2_PLACEMENT_3D('',#22560,#18443,#18444);
#16219=AXIS2_PLACEMENT_3D('',#22566,#18448,#18449);
#16220=AXIS2_PLACEMENT_3D('',#22568,#18450,#18451);
#16221=AXIS2_PLACEMENT_3D('',#22571,#18453,#18454);
#16222=AXIS2_PLACEMENT_3D('',#22572,#18455,#18456);
#16223=AXIS2_PLACEMENT_3D('',#22578,#18460,#18461);
#16224=AXIS2_PLACEMENT_3D('',#22584,#18465,#18466);
#16225=AXIS2_PLACEMENT_3D('',#22590,#18470,#18471);
#16226=AXIS2_PLACEMENT_3D('',#22596,#18475,#18476);
#16227=AXIS2_PLACEMENT_3D('',#22599,#18479,#18480);
#16228=AXIS2_PLACEMENT_3D('',#22600,#18481,#18482);
#16229=AXIS2_PLACEMENT_3D('',#22601,#18483,#18484);
#16230=AXIS2_PLACEMENT_3D('',#22603,#18485,#18486);
#16231=AXIS2_PLACEMENT_3D('',#22606,#18488,#18489);
#16232=AXIS2_PLACEMENT_3D('',#22607,#18490,#18491);
#16233=AXIS2_PLACEMENT_3D('',#22610,#18492,#18493);
#16234=AXIS2_PLACEMENT_3D('',#22614,#18495,#18496);
#16235=AXIS2_PLACEMENT_3D('',#22616,#18498,#18499);
#16236=AXIS2_PLACEMENT_3D('',#22618,#18500,#18501);
#16237=AXIS2_PLACEMENT_3D('',#22621,#18503,#18504);
#16238=AXIS2_PLACEMENT_3D('',#22622,#18505,#18506);
#16239=AXIS2_PLACEMENT_3D('',#22630,#18511,#18512);
#16240=AXIS2_PLACEMENT_3D('',#22638,#18517,#18518);
#16241=AXIS2_PLACEMENT_3D('',#22640,#18520,#18521);
#16242=AXIS2_PLACEMENT_3D('',#22642,#18523,#18524);
#16243=AXIS2_PLACEMENT_3D('',#22644,#18526,#18527);
#16244=AXIS2_PLACEMENT_3D('',#22645,#18528,#18529);
#16245=AXIS2_PLACEMENT_3D('',#22647,#18530,#18531);
#16246=AXIS2_PLACEMENT_3D('',#22650,#18533,#18534);
#16247=AXIS2_PLACEMENT_3D('',#22651,#18535,#18536);
#16248=AXIS2_PLACEMENT_3D('',#22654,#18537,#18538);
#16249=AXIS2_PLACEMENT_3D('',#22658,#18540,#18541);
#16250=AXIS2_PLACEMENT_3D('',#22660,#18543,#18544);
#16251=AXIS2_PLACEMENT_3D('',#22662,#18545,#18546);
#16252=AXIS2_PLACEMENT_3D('',#22664,#18547,#18548);
#16253=AXIS2_PLACEMENT_3D('',#22666,#18550,#18551);
#16254=AXIS2_PLACEMENT_3D('',#22674,#18556,#18557);
#16255=AXIS2_PLACEMENT_3D('',#22682,#18562,#18563);
#16256=AXIS2_PLACEMENT_3D('',#22684,#18565,#18566);
#16257=AXIS2_PLACEMENT_3D('',#22686,#18568,#18569);
#16258=AXIS2_PLACEMENT_3D('',#22688,#18571,#18572);
#16259=AXIS2_PLACEMENT_3D('',#22689,#18573,#18574);
#16260=AXIS2_PLACEMENT_3D('',#22692,#18575,#18576);
#16261=AXIS2_PLACEMENT_3D('',#22694,#18577,#18578);
#16262=AXIS2_PLACEMENT_3D('',#22695,#18579,#18580);
#16263=AXIS2_PLACEMENT_3D('',#22696,#18581,#18582);
#16264=AXIS2_PLACEMENT_3D('',#22697,#18583,#18584);
#16265=AXIS2_PLACEMENT_3D('',#22699,#18585,#18586);
#16266=AXIS2_PLACEMENT_3D('',#22701,#18587,#18588);
#16267=AXIS2_PLACEMENT_3D('',#22703,#18589,#18590);
#16268=AXIS2_PLACEMENT_3D('',#22704,#18591,#18592);
#16269=AXIS2_PLACEMENT_3D('',#22705,#18593,#18594);
#16270=AXIS2_PLACEMENT_3D('',#22708,#18596,#18597);
#16271=AXIS2_PLACEMENT_3D('',#22709,#18598,#18599);
#16272=AXIS2_PLACEMENT_3D('',#22711,#18601,#18602);
#16273=AXIS2_PLACEMENT_3D('',#22713,#18603,#18604);
#16274=AXIS2_PLACEMENT_3D('',#22715,#18606,#18607);
#16275=AXIS2_PLACEMENT_3D('',#22716,#18608,#18609);
#16276=AXIS2_PLACEMENT_3D('',#22717,#18610,#18611);
#16277=AXIS2_PLACEMENT_3D('',#22718,#18612,#18613);
#16278=AXIS2_PLACEMENT_3D('',#22720,#18614,#18615);
#16279=AXIS2_PLACEMENT_3D('',#22723,#18617,#18618);
#16280=AXIS2_PLACEMENT_3D('',#22724,#18619,#18620);
#16281=AXIS2_PLACEMENT_3D('',#22726,#18621,#18622);
#16282=AXIS2_PLACEMENT_3D('',#22728,#18624,#18625);
#16283=AXIS2_PLACEMENT_3D('',#22743,#18629,#18630);
#16284=AXIS2_PLACEMENT_3D('',#22755,#18633,#18634);
#16285=AXIS2_PLACEMENT_3D('',#22767,#18637,#18638);
#16286=AXIS2_PLACEMENT_3D('',#22779,#18641,#18642);
#16287=AXIS2_PLACEMENT_3D('',#22791,#18645,#18646);
#16288=AXIS2_PLACEMENT_3D('',#22800,#18648,#18649);
#16289=AXIS2_PLACEMENT_3D('',#22801,#18650,#18651);
#16290=AXIS2_PLACEMENT_3D('',#22802,#18652,#18653);
#16291=AXIS2_PLACEMENT_3D('',#22803,#18654,#18655);
#16292=AXIS2_PLACEMENT_3D('',#22804,#18656,#18657);
#16293=AXIS2_PLACEMENT_3D('',#22805,#18658,#18659);
#16294=AXIS2_PLACEMENT_3D('',#22806,#18660,#18661);
#16295=AXIS2_PLACEMENT_3D('',#22807,#18662,#18663);
#16296=AXIS2_PLACEMENT_3D('',#22808,#18664,#18665);
#16297=AXIS2_PLACEMENT_3D('',#22809,#18666,#18667);
#16298=AXIS2_PLACEMENT_3D('',#22810,#18668,#18669);
#16299=AXIS2_PLACEMENT_3D('',#22811,#18670,#18671);
#16300=AXIS2_PLACEMENT_3D('',#22812,#18672,#18673);
#16301=AXIS2_PLACEMENT_3D('',#22813,#18674,#18675);
#16302=AXIS2_PLACEMENT_3D('',#22814,#18676,#18677);
#16303=AXIS2_PLACEMENT_3D('',#22815,#18678,#18679);
#16304=AXIS2_PLACEMENT_3D('',#22816,#18680,#18681);
#16305=AXIS2_PLACEMENT_3D('',#22818,#18682,#18683);
#16306=AXIS2_PLACEMENT_3D('',#22821,#18685,#18686);
#16307=AXIS2_PLACEMENT_3D('',#22822,#18687,#18688);
#16308=AXIS2_PLACEMENT_3D('',#22824,#18689,#18690);
#16309=AXIS2_PLACEMENT_3D('',#22826,#18692,#18693);
#16310=AXIS2_PLACEMENT_3D('',#22841,#18697,#18698);
#16311=AXIS2_PLACEMENT_3D('',#22853,#18701,#18702);
#16312=AXIS2_PLACEMENT_3D('',#22865,#18705,#18706);
#16313=AXIS2_PLACEMENT_3D('',#22877,#18709,#18710);
#16314=AXIS2_PLACEMENT_3D('',#22889,#18713,#18714);
#16315=AXIS2_PLACEMENT_3D('',#22898,#18716,#18717);
#16316=AXIS2_PLACEMENT_3D('',#22899,#18718,#18719);
#16317=AXIS2_PLACEMENT_3D('',#22900,#18720,#18721);
#16318=AXIS2_PLACEMENT_3D('',#22901,#18722,#18723);
#16319=AXIS2_PLACEMENT_3D('',#22902,#18724,#18725);
#16320=AXIS2_PLACEMENT_3D('',#22903,#18726,#18727);
#16321=AXIS2_PLACEMENT_3D('',#22904,#18728,#18729);
#16322=AXIS2_PLACEMENT_3D('',#22905,#18730,#18731);
#16323=AXIS2_PLACEMENT_3D('',#22906,#18732,#18733);
#16324=AXIS2_PLACEMENT_3D('',#22907,#18734,#18735);
#16325=AXIS2_PLACEMENT_3D('',#22908,#18736,#18737);
#16326=AXIS2_PLACEMENT_3D('',#22909,#18738,#18739);
#16327=AXIS2_PLACEMENT_3D('',#22910,#18740,#18741);
#16328=AXIS2_PLACEMENT_3D('',#22911,#18742,#18743);
#16329=AXIS2_PLACEMENT_3D('',#22912,#18744,#18745);
#16330=AXIS2_PLACEMENT_3D('',#22913,#18746,#18747);
#16331=AXIS2_PLACEMENT_3D('',#22914,#18748,#18749);
#16332=AXIS2_PLACEMENT_3D('',#22916,#18750,#18751);
#16333=AXIS2_PLACEMENT_3D('',#22920,#18753,#18754);
#16334=AXIS2_PLACEMENT_3D('',#22921,#18755,#18756);
#16335=AXIS2_PLACEMENT_3D('',#22922,#18757,#18758);
#16336=AXIS2_PLACEMENT_3D('',#22925,#18759,#18760);
#16337=AXIS2_PLACEMENT_3D('',#22927,#18762,#18763);
#16338=AXIS2_PLACEMENT_3D('',#22928,#18764,#18765);
#16339=AXIS2_PLACEMENT_3D('',#22930,#18766,#18767);
#16340=AXIS2_PLACEMENT_3D('',#22933,#18769,#18770);
#16341=AXIS2_PLACEMENT_3D('',#22934,#18771,#18772);
#16342=AXIS2_PLACEMENT_3D('',#22936,#18774,#18775);
#16343=AXIS2_PLACEMENT_3D('',#22957,#18778,#18779);
#16344=AXIS2_PLACEMENT_3D('',#22975,#18781,#18782);
#16345=AXIS2_PLACEMENT_3D('',#22993,#18784,#18785);
#16346=AXIS2_PLACEMENT_3D('',#23011,#18787,#18788);
#16347=AXIS2_PLACEMENT_3D('',#23029,#18790,#18791);
#16348=AXIS2_PLACEMENT_3D('',#23044,#18792,#18793);
#16349=AXIS2_PLACEMENT_3D('',#23045,#18794,#18795);
#16350=AXIS2_PLACEMENT_3D('',#23046,#18796,#18797);
#16351=AXIS2_PLACEMENT_3D('',#23047,#18798,#18799);
#16352=AXIS2_PLACEMENT_3D('',#23048,#18800,#18801);
#16353=AXIS2_PLACEMENT_3D('',#23049,#18802,#18803);
#16354=AXIS2_PLACEMENT_3D('',#23050,#18804,#18805);
#16355=AXIS2_PLACEMENT_3D('',#23051,#18806,#18807);
#16356=AXIS2_PLACEMENT_3D('',#23052,#18808,#18809);
#16357=AXIS2_PLACEMENT_3D('',#23053,#18810,#18811);
#16358=AXIS2_PLACEMENT_3D('',#23054,#18812,#18813);
#16359=AXIS2_PLACEMENT_3D('',#23055,#18814,#18815);
#16360=AXIS2_PLACEMENT_3D('',#23056,#18816,#18817);
#16361=AXIS2_PLACEMENT_3D('',#23057,#18818,#18819);
#16362=AXIS2_PLACEMENT_3D('',#23058,#18820,#18821);
#16363=AXIS2_PLACEMENT_3D('',#23059,#18822,#18823);
#16364=AXIS2_PLACEMENT_3D('',#23060,#18824,#18825);
#16365=AXIS2_PLACEMENT_3D('',#23061,#18826,#18827);
#16366=AXIS2_PLACEMENT_3D('',#23062,#18828,#18829);
#16367=AXIS2_PLACEMENT_3D('',#23063,#18830,#18831);
#16368=AXIS2_PLACEMENT_3D('',#23064,#18832,#18833);
#16369=AXIS2_PLACEMENT_3D('',#23065,#18834,#18835);
#16370=AXIS2_PLACEMENT_3D('',#23066,#18836,#18837);
#16371=AXIS2_PLACEMENT_3D('',#23067,#18838,#18839);
#16372=AXIS2_PLACEMENT_3D('',#23068,#18840,#18841);
#16373=AXIS2_PLACEMENT_3D('',#23069,#18842,#18843);
#16374=AXIS2_PLACEMENT_3D('',#23070,#18844,#18845);
#16375=AXIS2_PLACEMENT_3D('',#23071,#18846,#18847);
#16376=AXIS2_PLACEMENT_3D('',#23088,#18849,#18850);
#16377=AXIS2_PLACEMENT_3D('',#23094,#18851,#18852);
#16378=AXIS2_PLACEMENT_3D('',#23140,#18854,#18855);
#16379=AXIS2_PLACEMENT_3D('',#23186,#18857,#18858);
#16380=AXIS2_PLACEMENT_3D('',#23232,#18860,#18861);
#16381=AXIS2_PLACEMENT_3D('',#23278,#18863,#18864);
#16382=AXIS2_PLACEMENT_3D('',#23324,#18866,#18867);
#16383=AXIS2_PLACEMENT_3D('',#23370,#18869,#18870);
#16384=AXIS2_PLACEMENT_3D('',#23416,#18872,#18873);
#16385=AXIS2_PLACEMENT_3D('',#23462,#18875,#18876);
#16386=AXIS2_PLACEMENT_3D('',#23508,#18878,#18879);
#16387=AXIS2_PLACEMENT_3D('',#23554,#18881,#18882);
#16388=AXIS2_PLACEMENT_3D('',#23600,#18884,#18885);
#16389=AXIS2_PLACEMENT_3D('',#23646,#18887,#18888);
#16390=AXIS2_PLACEMENT_3D('',#23692,#18890,#18891);
#16391=AXIS2_PLACEMENT_3D('',#23738,#18893,#18894);
#16392=AXIS2_PLACEMENT_3D('',#23784,#18896,#18897);
#16393=AXIS2_PLACEMENT_3D('',#23830,#18899,#18900);
#16394=AXIS2_PLACEMENT_3D('',#23876,#18902,#18903);
#16395=AXIS2_PLACEMENT_3D('',#23922,#18905,#18906);
#16396=AXIS2_PLACEMENT_3D('',#23968,#18908,#18909);
#16397=AXIS2_PLACEMENT_3D('',#24014,#18911,#18912);
#16398=AXIS2_PLACEMENT_3D('',#24060,#18914,#18915);
#16399=AXIS2_PLACEMENT_3D('',#24583,#18919,#18920);
#16400=AXIS2_PLACEMENT_3D('',#24659,#18922,#18923);
#16401=AXIS2_PLACEMENT_3D('',#24735,#18925,#18926);
#16402=AXIS2_PLACEMENT_3D('',#24811,#18928,#18929);
#16403=AXIS2_PLACEMENT_3D('',#24887,#18931,#18932);
#16404=AXIS2_PLACEMENT_3D('',#24963,#18934,#18935);
#16405=AXIS2_PLACEMENT_3D('',#25041,#18937,#18938);
#16406=AXIS2_PLACEMENT_3D('',#25117,#18940,#18941);
#16407=AXIS2_PLACEMENT_3D('',#25193,#18943,#18944);
#16408=AXIS2_PLACEMENT_3D('',#25271,#18946,#18947);
#16409=AXIS2_PLACEMENT_3D('',#25347,#18949,#18950);
#16410=AXIS2_PLACEMENT_3D('',#25423,#18952,#18953);
#16411=AXIS2_PLACEMENT_3D('',#25499,#18955,#18956);
#16412=AXIS2_PLACEMENT_3D('',#25575,#18958,#18959);
#16413=AXIS2_PLACEMENT_3D('',#25651,#18961,#18962);
#16414=AXIS2_PLACEMENT_3D('',#25729,#18964,#18965);
#16415=AXIS2_PLACEMENT_3D('',#25805,#18967,#18968);
#16416=AXIS2_PLACEMENT_3D('',#25883,#18970,#18971);
#16417=AXIS2_PLACEMENT_3D('',#25959,#18973,#18974);
#16418=AXIS2_PLACEMENT_3D('',#26035,#18976,#18977);
#16419=AXIS2_PLACEMENT_3D('',#26040,#18979,#18980);
#16420=AXIS2_PLACEMENT_3D('',#26111,#18981,#18982);
#16421=AXIS2_PLACEMENT_3D('',#26114,#18983,#18984);
#16422=AXIS2_PLACEMENT_3D('',#26116,#18985,#18986);
#16423=AXIS2_PLACEMENT_3D('',#26118,#18987,#18988);
#16424=AXIS2_PLACEMENT_3D('',#26119,#18989,#18990);
#16425=AXIS2_PLACEMENT_3D('',#26120,#18991,#18992);
#16426=AXIS2_PLACEMENT_3D('',#26123,#18993,#18994);
#16427=AXIS2_PLACEMENT_3D('',#26125,#18995,#18996);
#16428=AXIS2_PLACEMENT_3D('',#26127,#18997,#18998);
#16429=AXIS2_PLACEMENT_3D('',#26128,#18999,#19000);
#16430=AXIS2_PLACEMENT_3D('',#26129,#19001,#19002);
#16431=AXIS2_PLACEMENT_3D('',#26131,#19003,#19004);
#16432=AXIS2_PLACEMENT_3D('',#26134,#19006,#19007);
#16433=AXIS2_PLACEMENT_3D('',#26135,#19008,#19009);
#16434=AXIS2_PLACEMENT_3D('',#26270,#19010,#19011);
#16435=AXIS2_PLACEMENT_3D('',#26286,#19012,#19013);
#16436=AXIS2_PLACEMENT_3D('',#26308,#19015,#19016);
#16437=AXIS2_PLACEMENT_3D('',#26327,#19017,#19018);
#16438=AXIS2_PLACEMENT_3D('',#26334,#19019,#19020);
#16439=AXIS2_PLACEMENT_3D('',#26449,#19021,#19022);
#16440=AXIS2_PLACEMENT_3D('',#26561,#19023,#19024);
#16441=AXIS2_PLACEMENT_3D('',#26562,#19025,#19026);
#16442=AXIS2_PLACEMENT_3D('',#27447,#19030,#19031);
#16443=AXIS2_PLACEMENT_3D('',#28364,#19032,#19033);
#16444=AXIS2_PLACEMENT_3D('',#28548,#19034,#19035);
#16445=AXIS2_PLACEMENT_3D('',#28632,#19036,#19037);
#16446=AXIS2_PLACEMENT_3D('',#28816,#19038,#19039);
#16447=AXIS2_PLACEMENT_3D('',#28907,#19040,#19041);
#16448=AXIS2_PLACEMENT_3D('',#28950,#19042,#19043);
#16449=AXIS2_PLACEMENT_3D('',#29047,#19044,#19045);
#16450=AXIS2_PLACEMENT_3D('',#29090,#19046,#19047);
#16451=AXIS2_PLACEMENT_3D('',#29139,#19048,#19049);
#16452=AXIS2_PLACEMENT_3D('',#29140,#19050,#19051);
#16453=AXIS2_PLACEMENT_3D('',#29161,#19053,#19054);
#16454=AXIS2_PLACEMENT_3D('',#29183,#19055,#19056);
#16455=AXIS2_PLACEMENT_3D('',#29229,#19058,#19059);
#16456=AXIS2_PLACEMENT_3D('',#29275,#19061,#19062);
#16457=AXIS2_PLACEMENT_3D('',#29321,#19064,#19065);
#16458=AXIS2_PLACEMENT_3D('',#29342,#19067,#19068);
#16459=AXIS2_PLACEMENT_3D('',#29362,#19069,#19070);
#16460=AXIS2_PLACEMENT_3D('',#29367,#19072,#19073);
#16461=AXIS2_PLACEMENT_3D('',#29376,#19074,#19075);
#16462=AXIS2_PLACEMENT_3D('',#29417,#19077,#19078);
#16463=AXIS2_PLACEMENT_3D('',#29454,#19079,#19080);
#16464=AXIS2_PLACEMENT_3D('',#29530,#19082,#19083);
#16465=AXIS2_PLACEMENT_3D('',#29606,#19085,#19086);
#16466=AXIS2_PLACEMENT_3D('',#29682,#19088,#19089);
#16467=AXIS2_PLACEMENT_3D('',#29706,#19091,#19092);
#16468=AXIS2_PLACEMENT_3D('',#29729,#19093,#19094);
#16469=AXIS2_PLACEMENT_3D('',#29731,#19095,#19096);
#16470=AXIS2_PLACEMENT_3D('',#29734,#19098,#19099);
#16471=AXIS2_PLACEMENT_3D('',#29735,#19100,#19101);
#16472=AXIS2_PLACEMENT_3D('',#29738,#19102,#19103);
#16473=AXIS2_PLACEMENT_3D('',#29740,#19105,#19106);
#16474=AXIS2_PLACEMENT_3D('',#29741,#19107,#19108);
#16475=AXIS2_PLACEMENT_3D('',#29745,#19110,#19111);
#16476=AXIS2_PLACEMENT_3D('',#29747,#19112,#19113);
#16477=AXIS2_PLACEMENT_3D('',#29769,#19114,#19115);
#16478=AXIS2_PLACEMENT_3D('',#29770,#19116,#19117);
#16479=AXIS2_PLACEMENT_3D('',#29771,#19118,#19119);
#16480=AXIS2_PLACEMENT_3D('',#29844,#19120,#19121);
#16481=AXIS2_PLACEMENT_3D('',#29849,#19122,#19123);
#16482=AXIS2_PLACEMENT_3D('',#29850,#19124,#19125);
#16483=AXIS2_PLACEMENT_3D('',#29852,#19126,#19127);
#16484=AXIS2_PLACEMENT_3D('',#29872,#19132,#19133);
#16485=AXIS2_PLACEMENT_3D('',#29878,#19134,#19135);
#16486=AXIS2_PLACEMENT_3D('',#29896,#19139,#19140);
#16487=AXIS2_PLACEMENT_3D('',#29897,#19141,#19142);
#16488=AXIS2_PLACEMENT_3D('',#29899,#19143,#19144);
#16489=AXIS2_PLACEMENT_3D('',#29903,#19146,#19147);
#16490=AXIS2_PLACEMENT_3D('',#29907,#19149,#19150);
#16491=AXIS2_PLACEMENT_3D('',#29911,#19152,#19153);
#16492=AXIS2_PLACEMENT_3D('',#29914,#19155,#19156);
#16493=AXIS2_PLACEMENT_3D('',#29951,#19157,#19158);
#16494=AXIS2_PLACEMENT_3D('',#29953,#19159,#19160);
#16495=AXIS2_PLACEMENT_3D('',#29957,#19162,#19163);
#16496=AXIS2_PLACEMENT_3D('',#29961,#19165,#19166);
#16497=AXIS2_PLACEMENT_3D('',#29965,#19168,#19169);
#16498=AXIS2_PLACEMENT_3D('',#29968,#19171,#19172);
#16499=AXIS2_PLACEMENT_3D('',#29969,#19173,#19174);
#16500=AXIS2_PLACEMENT_3D('',#30004,#19175,#19176);
#16501=AXIS2_PLACEMENT_3D('',#30020,#19178,#19179);
#16502=AXIS2_PLACEMENT_3D('',#30036,#19181,#19182);
#16503=AXIS2_PLACEMENT_3D('',#30052,#19184,#19185);
#16504=AXIS2_PLACEMENT_3D('',#30065,#19186,#19187);
#16505=AXIS2_PLACEMENT_3D('',#30066,#19188,#19189);
#16506=AXIS2_PLACEMENT_3D('',#30067,#19190,#19191);
#16507=AXIS2_PLACEMENT_3D('',#30068,#19192,#19193);
#16508=AXIS2_PLACEMENT_3D('',#30069,#19194,#19195);
#16509=AXIS2_PLACEMENT_3D('',#30070,#19196,#19197);
#16510=AXIS2_PLACEMENT_3D('',#30071,#19198,#19199);
#16511=AXIS2_PLACEMENT_3D('',#30072,#19200,#19201);
#16512=AXIS2_PLACEMENT_3D('',#30073,#19202,#19203);
#16513=AXIS2_PLACEMENT_3D('',#30074,#19204,#19205);
#16514=AXIS2_PLACEMENT_3D('',#30075,#19206,#19207);
#16515=AXIS2_PLACEMENT_3D('',#30076,#19208,#19209);
#16516=AXIS2_PLACEMENT_3D('',#30372,#19210,#19211);
#16517=AXIS2_PLACEMENT_3D('',#30668,#19212,#19213);
#16518=AXIS2_PLACEMENT_3D('',#30669,#19214,#19215);
#16519=AXIS2_PLACEMENT_3D('',#30670,#19216,#19217);
#16520=AXIS2_PLACEMENT_3D('',#30671,#19218,#19219);
#16521=AXIS2_PLACEMENT_3D('',#30673,#19220,#19221);
#16522=AXIS2_PLACEMENT_3D('',#30676,#19223,#19224);
#16523=AXIS2_PLACEMENT_3D('',#30677,#19225,#19226);
#16524=AXIS2_PLACEMENT_3D('',#30679,#19227,#19228);
#16525=AXIS2_PLACEMENT_3D('',#30682,#19230,#19231);
#16526=AXIS2_PLACEMENT_3D('',#30683,#19232,#19233);
#16527=AXIS2_PLACEMENT_3D('',#30684,#19234,#19235);
#16528=AXIS2_PLACEMENT_3D('',#30685,#19236,#19237);
#16529=AXIS2_PLACEMENT_3D('',#30686,#19238,#19239);
#16530=AXIS2_PLACEMENT_3D('',#30687,#19240,#19241);
#16531=AXIS2_PLACEMENT_3D('',#30688,#19242,#19243);
#16532=AXIS2_PLACEMENT_3D('',#30689,#19244,#19245);
#16533=AXIS2_PLACEMENT_3D('',#30690,#19246,#19247);
#16534=AXIS2_PLACEMENT_3D('',#30691,#19248,#19249);
#16535=AXIS2_PLACEMENT_3D('',#30692,#19250,#19251);
#16536=AXIS2_PLACEMENT_3D('',#30693,#19252,#19253);
#16537=AXIS2_PLACEMENT_3D('',#30694,#19254,#19255);
#16538=AXIS2_PLACEMENT_3D('',#30695,#19256,#19257);
#16539=AXIS2_PLACEMENT_3D('',#30696,#19258,#19259);
#16540=AXIS2_PLACEMENT_3D('',#30697,#19260,#19261);
#16541=AXIS2_PLACEMENT_3D('',#30698,#19262,#19263);
#16542=AXIS2_PLACEMENT_3D('',#30699,#19264,#19265);
#16543=AXIS2_PLACEMENT_3D('',#30700,#19266,#19267);
#16544=AXIS2_PLACEMENT_3D('',#30701,#19268,#19269);
#16545=AXIS2_PLACEMENT_3D('',#30702,#19270,#19271);
#16546=AXIS2_PLACEMENT_3D('',#30703,#19272,#19273);
#16547=AXIS2_PLACEMENT_3D('',#30704,#19274,#19275);
#16548=AXIS2_PLACEMENT_3D('',#30705,#19276,#19277);
#16549=AXIS2_PLACEMENT_3D('',#30706,#19278,#19279);
#16550=AXIS2_PLACEMENT_3D('',#30715,#19284,#19285);
#16551=AXIS2_PLACEMENT_3D('',#30721,#19289,#19290);
#16552=AXIS2_PLACEMENT_3D('',#30727,#19294,#19295);
#16553=AXIS2_PLACEMENT_3D('',#30730,#19298,#19299);
#16554=AXIS2_PLACEMENT_3D('',#30731,#19300,#19301);
#16555=AXIS2_PLACEMENT_3D('',#30732,#19302,#19303);
#16556=AXIS2_PLACEMENT_3D('',#30734,#19304,#19305);
#16557=AXIS2_PLACEMENT_3D('',#30737,#19307,#19308);
#16558=AXIS2_PLACEMENT_3D('',#30738,#19309,#19310);
#16559=AXIS2_PLACEMENT_3D('',#30749,#19315,#19316);
#16560=AXIS2_PLACEMENT_3D('',#30751,#19318,#19319);
#16561=AXIS2_PLACEMENT_3D('',#30758,#19322,#19323);
#16562=AXIS2_PLACEMENT_3D('',#30764,#19327,#19328);
#16563=AXIS2_PLACEMENT_3D('',#30767,#19331,#19332);
#16564=AXIS2_PLACEMENT_3D('',#30769,#19334,#19335);
#16565=AXIS2_PLACEMENT_3D('',#30771,#19337,#19338);
#16566=AXIS2_PLACEMENT_3D('',#30773,#19340,#19341);
#16567=AXIS2_PLACEMENT_3D('',#30775,#19343,#19344);
#16568=AXIS2_PLACEMENT_3D('',#30776,#19345,#19346);
#16569=AXIS2_PLACEMENT_3D('',#30778,#19347,#19348);
#16570=AXIS2_PLACEMENT_3D('',#30781,#19350,#19351);
#16571=AXIS2_PLACEMENT_3D('',#30782,#19352,#19353);
#16572=AXIS2_PLACEMENT_3D('',#30789,#19356,#19357);
#16573=AXIS2_PLACEMENT_3D('',#30795,#19361,#19362);
#16574=AXIS2_PLACEMENT_3D('',#30806,#19367,#19368);
#16575=AXIS2_PLACEMENT_3D('',#30808,#19370,#19371);
#16576=AXIS2_PLACEMENT_3D('',#30811,#19374,#19375);
#16577=AXIS2_PLACEMENT_3D('',#30813,#19377,#19378);
#16578=AXIS2_PLACEMENT_3D('',#30815,#19380,#19381);
#16579=AXIS2_PLACEMENT_3D('',#30817,#19383,#19384);
#16580=AXIS2_PLACEMENT_3D('',#30819,#19386,#19387);
#16581=AXIS2_PLACEMENT_3D('',#30820,#19388,#19389);
#16582=AXIS2_PLACEMENT_3D('',#30822,#19390,#19391);
#16583=AXIS2_PLACEMENT_3D('',#30825,#19393,#19394);
#16584=AXIS2_PLACEMENT_3D('',#30826,#19395,#19396);
#16585=AXIS2_PLACEMENT_3D('',#30828,#19397,#19398);
#16586=AXIS2_PLACEMENT_3D('',#30831,#19400,#19401);
#16587=AXIS2_PLACEMENT_3D('',#30832,#19402,#19403);
#16588=AXIS2_PLACEMENT_3D('',#30834,#19404,#19405);
#16589=AXIS2_PLACEMENT_3D('',#30837,#19407,#19408);
#16590=AXIS2_PLACEMENT_3D('',#30838,#19409,#19410);
#16591=AXIS2_PLACEMENT_3D('',#30840,#19411,#19412);
#16592=AXIS2_PLACEMENT_3D('',#30843,#19414,#19415);
#16593=AXIS2_PLACEMENT_3D('',#30844,#19416,#19417);
#16594=AXIS2_PLACEMENT_3D('',#30846,#19418,#19419);
#16595=AXIS2_PLACEMENT_3D('',#30849,#19421,#19422);
#16596=AXIS2_PLACEMENT_3D('',#30850,#19423,#19424);
#16597=AXIS2_PLACEMENT_3D('',#30867,#19433,#19434);
#16598=AXIS2_PLACEMENT_3D('',#30884,#19443,#19444);
#16599=AXIS2_PLACEMENT_3D('',#30887,#19447,#19448);
#16600=AXIS2_PLACEMENT_3D('',#30889,#19450,#19451);
#16601=AXIS2_PLACEMENT_3D('',#30891,#19453,#19454);
#16602=AXIS2_PLACEMENT_3D('',#30893,#19456,#19457);
#16603=AXIS2_PLACEMENT_3D('',#30895,#19459,#19460);
#16604=AXIS2_PLACEMENT_3D('',#30897,#19462,#19463);
#16605=AXIS2_PLACEMENT_3D('',#30899,#19465,#19466);
#16606=AXIS2_PLACEMENT_3D('',#30900,#19467,#19468);
#16607=AXIS2_PLACEMENT_3D('',#30909,#19473,#19474);
#16608=AXIS2_PLACEMENT_3D('',#30915,#19478,#19479);
#16609=AXIS2_PLACEMENT_3D('',#30921,#19483,#19484);
#16610=AXIS2_PLACEMENT_3D('',#30924,#19487,#19488);
#16611=AXIS2_PLACEMENT_3D('',#30925,#19489,#19490);
#16612=AXIS2_PLACEMENT_3D('',#30926,#19491,#19492);
#16613=AXIS2_PLACEMENT_3D('',#30935,#19497,#19498);
#16614=AXIS2_PLACEMENT_3D('',#30941,#19502,#19503);
#16615=AXIS2_PLACEMENT_3D('',#30947,#19507,#19508);
#16616=AXIS2_PLACEMENT_3D('',#30950,#19511,#19512);
#16617=AXIS2_PLACEMENT_3D('',#30951,#19513,#19514);
#16618=AXIS2_PLACEMENT_3D('',#30952,#19515,#19516);
#16619=AXIS2_PLACEMENT_3D('',#30961,#19521,#19522);
#16620=AXIS2_PLACEMENT_3D('',#30967,#19526,#19527);
#16621=AXIS2_PLACEMENT_3D('',#30973,#19531,#19532);
#16622=AXIS2_PLACEMENT_3D('',#30979,#19536,#19537);
#16623=AXIS2_PLACEMENT_3D('',#30985,#19541,#19542);
#16624=AXIS2_PLACEMENT_3D('',#30988,#19545,#19546);
#16625=AXIS2_PLACEMENT_3D('',#30989,#19547,#19548);
#16626=AXIS2_PLACEMENT_3D('',#30990,#19549,#19550);
#16627=AXIS2_PLACEMENT_3D('',#30992,#19551,#19552);
#16628=AXIS2_PLACEMENT_3D('',#30995,#19554,#19555);
#16629=AXIS2_PLACEMENT_3D('',#30996,#19556,#19557);
#16630=AXIS2_PLACEMENT_3D('',#30998,#19558,#19559);
#16631=AXIS2_PLACEMENT_3D('',#31001,#19561,#19562);
#16632=AXIS2_PLACEMENT_3D('',#31002,#19563,#19564);
#16633=AXIS2_PLACEMENT_3D('',#31004,#19565,#19566);
#16634=AXIS2_PLACEMENT_3D('',#31007,#19568,#19569);
#16635=AXIS2_PLACEMENT_3D('',#31008,#19570,#19571);
#16636=AXIS2_PLACEMENT_3D('',#31017,#19576,#19577);
#16637=AXIS2_PLACEMENT_3D('',#31026,#19582,#19583);
#16638=AXIS2_PLACEMENT_3D('',#31029,#19586,#19587);
#16639=AXIS2_PLACEMENT_3D('',#31031,#19589,#19590);
#16640=AXIS2_PLACEMENT_3D('',#31033,#19592,#19593);
#16641=AXIS2_PLACEMENT_3D('',#31034,#19594,#19595);
#16642=AXIS2_PLACEMENT_3D('',#31036,#19596,#19597);
#16643=AXIS2_PLACEMENT_3D('',#31039,#19599,#19600);
#16644=AXIS2_PLACEMENT_3D('',#31040,#19601,#19602);
#16645=AXIS2_PLACEMENT_3D('',#31042,#19603,#19604);
#16646=AXIS2_PLACEMENT_3D('',#31045,#19606,#19607);
#16647=AXIS2_PLACEMENT_3D('',#31046,#19608,#19609);
#16648=AXIS2_PLACEMENT_3D('',#31048,#19610,#19611);
#16649=AXIS2_PLACEMENT_3D('',#31051,#19613,#19614);
#16650=AXIS2_PLACEMENT_3D('',#31052,#19615,#19616);
#16651=AXIS2_PLACEMENT_3D('',#31061,#19621,#19622);
#16652=AXIS2_PLACEMENT_3D('',#31070,#19627,#19628);
#16653=AXIS2_PLACEMENT_3D('',#31073,#19631,#19632);
#16654=AXIS2_PLACEMENT_3D('',#31075,#19634,#19635);
#16655=AXIS2_PLACEMENT_3D('',#31077,#19637,#19638);
#16656=AXIS2_PLACEMENT_3D('',#31078,#19639,#19640);
#16657=AXIS2_PLACEMENT_3D('',#31080,#19641,#19642);
#16658=AXIS2_PLACEMENT_3D('',#31083,#19644,#19645);
#16659=AXIS2_PLACEMENT_3D('',#31084,#19646,#19647);
#16660=AXIS2_PLACEMENT_3D('',#31086,#19648,#19649);
#16661=AXIS2_PLACEMENT_3D('',#31089,#19651,#19652);
#16662=AXIS2_PLACEMENT_3D('',#31090,#19653,#19654);
#16663=AXIS2_PLACEMENT_3D('',#31092,#19655,#19656);
#16664=AXIS2_PLACEMENT_3D('',#31095,#19658,#19659);
#16665=AXIS2_PLACEMENT_3D('',#31096,#19660,#19661);
#16666=AXIS2_PLACEMENT_3D('',#31105,#19666,#19667);
#16667=AXIS2_PLACEMENT_3D('',#31114,#19672,#19673);
#16668=AXIS2_PLACEMENT_3D('',#31117,#19676,#19677);
#16669=AXIS2_PLACEMENT_3D('',#31119,#19679,#19680);
#16670=AXIS2_PLACEMENT_3D('',#31121,#19682,#19683);
#16671=AXIS2_PLACEMENT_3D('',#31122,#19684,#19685);
#16672=AXIS2_PLACEMENT_3D('',#31124,#19686,#19687);
#16673=AXIS2_PLACEMENT_3D('',#31127,#19689,#19690);
#16674=AXIS2_PLACEMENT_3D('',#31128,#19691,#19692);
#16675=AXIS2_PLACEMENT_3D('',#31130,#19693,#19694);
#16676=AXIS2_PLACEMENT_3D('',#31133,#19696,#19697);
#16677=AXIS2_PLACEMENT_3D('',#31134,#19698,#19699);
#16678=AXIS2_PLACEMENT_3D('',#31136,#19700,#19701);
#16679=AXIS2_PLACEMENT_3D('',#31139,#19703,#19704);
#16680=AXIS2_PLACEMENT_3D('',#31140,#19705,#19706);
#16681=AXIS2_PLACEMENT_3D('',#31149,#19711,#19712);
#16682=AXIS2_PLACEMENT_3D('',#31158,#19717,#19718);
#16683=AXIS2_PLACEMENT_3D('',#31161,#19721,#19722);
#16684=AXIS2_PLACEMENT_3D('',#31163,#19724,#19725);
#16685=AXIS2_PLACEMENT_3D('',#31165,#19727,#19728);
#16686=AXIS2_PLACEMENT_3D('',#31166,#19729,#19730);
#16687=AXIS2_PLACEMENT_3D('',#31175,#19735,#19736);
#16688=AXIS2_PLACEMENT_3D('',#31181,#19740,#19741);
#16689=AXIS2_PLACEMENT_3D('',#31187,#19745,#19746);
#16690=AXIS2_PLACEMENT_3D('',#31190,#19749,#19750);
#16691=AXIS2_PLACEMENT_3D('',#31191,#19751,#19752);
#16692=AXIS2_PLACEMENT_3D('',#31192,#19753,#19754);
#16693=AXIS2_PLACEMENT_3D('',#31201,#19759,#19760);
#16694=AXIS2_PLACEMENT_3D('',#31207,#19764,#19765);
#16695=AXIS2_PLACEMENT_3D('',#31213,#19769,#19770);
#16696=AXIS2_PLACEMENT_3D('',#31216,#19773,#19774);
#16697=AXIS2_PLACEMENT_3D('',#31217,#19775,#19776);
#16698=AXIS2_PLACEMENT_3D('',#31218,#19777,#19778);
#16699=AXIS2_PLACEMENT_3D('',#31227,#19783,#19784);
#16700=AXIS2_PLACEMENT_3D('',#31233,#19788,#19789);
#16701=AXIS2_PLACEMENT_3D('',#31239,#19793,#19794);
#16702=AXIS2_PLACEMENT_3D('',#31242,#19797,#19798);
#16703=AXIS2_PLACEMENT_3D('',#31243,#19799,#19800);
#16704=AXIS2_PLACEMENT_3D('',#31244,#19801,#19802);
#16705=AXIS2_PLACEMENT_3D('',#31253,#19807,#19808);
#16706=AXIS2_PLACEMENT_3D('',#31259,#19812,#19813);
#16707=AXIS2_PLACEMENT_3D('',#31265,#19817,#19818);
#16708=AXIS2_PLACEMENT_3D('',#31268,#19821,#19822);
#16709=AXIS2_PLACEMENT_3D('',#31269,#19823,#19824);
#16710=AXIS2_PLACEMENT_3D('',#31270,#19825,#19826);
#16711=AXIS2_PLACEMENT_3D('',#31279,#19831,#19832);
#16712=AXIS2_PLACEMENT_3D('',#31285,#19836,#19837);
#16713=AXIS2_PLACEMENT_3D('',#31291,#19841,#19842);
#16714=AXIS2_PLACEMENT_3D('',#31294,#19845,#19846);
#16715=AXIS2_PLACEMENT_3D('',#31295,#19847,#19848);
#16716=AXIS2_PLACEMENT_3D('',#31296,#19849,#19850);
#16717=AXIS2_PLACEMENT_3D('',#31298,#19851,#19852);
#16718=AXIS2_PLACEMENT_3D('',#31301,#19854,#19855);
#16719=AXIS2_PLACEMENT_3D('',#31302,#19856,#19857);
#16720=AXIS2_PLACEMENT_3D('',#31304,#19858,#19859);
#16721=AXIS2_PLACEMENT_3D('',#31307,#19861,#19862);
#16722=AXIS2_PLACEMENT_3D('',#31308,#19863,#19864);
#16723=AXIS2_PLACEMENT_3D('',#31310,#19865,#19866);
#16724=AXIS2_PLACEMENT_3D('',#31313,#19868,#19869);
#16725=AXIS2_PLACEMENT_3D('',#31314,#19870,#19871);
#16726=AXIS2_PLACEMENT_3D('',#31316,#19872,#19873);
#16727=AXIS2_PLACEMENT_3D('',#31319,#19875,#19876);
#16728=AXIS2_PLACEMENT_3D('',#31320,#19877,#19878);
#16729=AXIS2_PLACEMENT_3D('',#31329,#19883,#19884);
#16730=AXIS2_PLACEMENT_3D('',#31338,#19889,#19890);
#16731=AXIS2_PLACEMENT_3D('',#31341,#19893,#19894);
#16732=AXIS2_PLACEMENT_3D('',#31343,#19896,#19897);
#16733=AXIS2_PLACEMENT_3D('',#31345,#19899,#19900);
#16734=AXIS2_PLACEMENT_3D('',#31346,#19901,#19902);
#16735=AXIS2_PLACEMENT_3D('',#31348,#19903,#19904);
#16736=AXIS2_PLACEMENT_3D('',#31351,#19906,#19907);
#16737=AXIS2_PLACEMENT_3D('',#31352,#19908,#19909);
#16738=AXIS2_PLACEMENT_3D('',#31354,#19910,#19911);
#16739=AXIS2_PLACEMENT_3D('',#31357,#19913,#19914);
#16740=AXIS2_PLACEMENT_3D('',#31358,#19915,#19916);
#16741=AXIS2_PLACEMENT_3D('',#31360,#19917,#19918);
#16742=AXIS2_PLACEMENT_3D('',#31363,#19920,#19921);
#16743=AXIS2_PLACEMENT_3D('',#31364,#19922,#19923);
#16744=AXIS2_PLACEMENT_3D('',#31366,#19924,#19925);
#16745=AXIS2_PLACEMENT_3D('',#31369,#19927,#19928);
#16746=AXIS2_PLACEMENT_3D('',#31370,#19929,#19930);
#16747=AXIS2_PLACEMENT_3D('',#31372,#19931,#19932);
#16748=AXIS2_PLACEMENT_3D('',#31375,#19934,#19935);
#16749=AXIS2_PLACEMENT_3D('',#31376,#19936,#19937);
#16750=AXIS2_PLACEMENT_3D('',#31378,#19938,#19939);
#16751=AXIS2_PLACEMENT_3D('',#31381,#19941,#19942);
#16752=AXIS2_PLACEMENT_3D('',#31382,#19943,#19944);
#16753=AXIS2_PLACEMENT_3D('',#31391,#19949,#19950);
#16754=AXIS2_PLACEMENT_3D('',#31397,#19954,#19955);
#16755=AXIS2_PLACEMENT_3D('',#31403,#19959,#19960);
#16756=AXIS2_PLACEMENT_3D('',#31406,#19963,#19964);
#16757=AXIS2_PLACEMENT_3D('',#31407,#19965,#19966);
#16758=AXIS2_PLACEMENT_3D('',#31408,#19967,#19968);
#16759=AXIS2_PLACEMENT_3D('',#31417,#19973,#19974);
#16760=AXIS2_PLACEMENT_3D('',#31423,#19978,#19979);
#16761=AXIS2_PLACEMENT_3D('',#31429,#19983,#19984);
#16762=AXIS2_PLACEMENT_3D('',#31435,#19988,#19989);
#16763=AXIS2_PLACEMENT_3D('',#31441,#19993,#19994);
#16764=AXIS2_PLACEMENT_3D('',#31447,#19998,#19999);
#16765=AXIS2_PLACEMENT_3D('',#31450,#20002,#20003);
#16766=AXIS2_PLACEMENT_3D('',#31451,#20004,#20005);
#16767=AXIS2_PLACEMENT_3D('',#31452,#20006,#20007);
#16768=AXIS2_PLACEMENT_3D('',#31461,#20012,#20013);
#16769=AXIS2_PLACEMENT_3D('',#31467,#20017,#20018);
#16770=AXIS2_PLACEMENT_3D('',#31473,#20022,#20023);
#16771=AXIS2_PLACEMENT_3D('',#31479,#20027,#20028);
#16772=AXIS2_PLACEMENT_3D('',#31485,#20032,#20033);
#16773=AXIS2_PLACEMENT_3D('',#31491,#20037,#20038);
#16774=AXIS2_PLACEMENT_3D('',#31494,#20041,#20042);
#16775=AXIS2_PLACEMENT_3D('',#31495,#20043,#20044);
#16776=AXIS2_PLACEMENT_3D('',#31496,#20045,#20046);
#16777=AXIS2_PLACEMENT_3D('',#31505,#20051,#20052);
#16778=AXIS2_PLACEMENT_3D('',#31511,#20056,#20057);
#16779=AXIS2_PLACEMENT_3D('',#31517,#20061,#20062);
#16780=AXIS2_PLACEMENT_3D('',#31523,#20066,#20067);
#16781=AXIS2_PLACEMENT_3D('',#31529,#20071,#20072);
#16782=AXIS2_PLACEMENT_3D('',#31535,#20076,#20077);
#16783=AXIS2_PLACEMENT_3D('',#31538,#20080,#20081);
#16784=AXIS2_PLACEMENT_3D('',#31539,#20082,#20083);
#16785=AXIS2_PLACEMENT_3D('',#31540,#20084,#20085);
#16786=AXIS2_PLACEMENT_3D('',#31549,#20090,#20091);
#16787=AXIS2_PLACEMENT_3D('',#31555,#20095,#20096);
#16788=AXIS2_PLACEMENT_3D('',#31561,#20100,#20101);
#16789=AXIS2_PLACEMENT_3D('',#31567,#20105,#20106);
#16790=AXIS2_PLACEMENT_3D('',#31573,#20110,#20111);
#16791=AXIS2_PLACEMENT_3D('',#31579,#20115,#20116);
#16792=AXIS2_PLACEMENT_3D('',#31582,#20119,#20120);
#16793=AXIS2_PLACEMENT_3D('',#31583,#20121,#20122);
#16794=AXIS2_PLACEMENT_3D('',#31584,#20123,#20124);
#16795=AXIS2_PLACEMENT_3D('',#31593,#20129,#20130);
#16796=AXIS2_PLACEMENT_3D('',#31599,#20134,#20135);
#16797=AXIS2_PLACEMENT_3D('',#31605,#20139,#20140);
#16798=AXIS2_PLACEMENT_3D('',#31611,#20144,#20145);
#16799=AXIS2_PLACEMENT_3D('',#31617,#20149,#20150);
#16800=AXIS2_PLACEMENT_3D('',#31623,#20154,#20155);
#16801=AXIS2_PLACEMENT_3D('',#31626,#20158,#20159);
#16802=AXIS2_PLACEMENT_3D('',#31627,#20160,#20161);
#16803=AXIS2_PLACEMENT_3D('',#31628,#20162,#20163);
#16804=AXIS2_PLACEMENT_3D('',#31637,#20168,#20169);
#16805=AXIS2_PLACEMENT_3D('',#31643,#20173,#20174);
#16806=AXIS2_PLACEMENT_3D('',#31649,#20178,#20179);
#16807=AXIS2_PLACEMENT_3D('',#31655,#20183,#20184);
#16808=AXIS2_PLACEMENT_3D('',#31661,#20188,#20189);
#16809=AXIS2_PLACEMENT_3D('',#31667,#20193,#20194);
#16810=AXIS2_PLACEMENT_3D('',#31670,#20197,#20198);
#16811=AXIS2_PLACEMENT_3D('',#31671,#20199,#20200);
#16812=AXIS2_PLACEMENT_3D('',#31672,#20201,#20202);
#16813=AXIS2_PLACEMENT_3D('',#31681,#20207,#20208);
#16814=AXIS2_PLACEMENT_3D('',#31687,#20212,#20213);
#16815=AXIS2_PLACEMENT_3D('',#31693,#20217,#20218);
#16816=AXIS2_PLACEMENT_3D('',#31699,#20222,#20223);
#16817=AXIS2_PLACEMENT_3D('',#31705,#20227,#20228);
#16818=AXIS2_PLACEMENT_3D('',#31711,#20232,#20233);
#16819=AXIS2_PLACEMENT_3D('',#31714,#20236,#20237);
#16820=AXIS2_PLACEMENT_3D('',#31715,#20238,#20239);
#16821=AXIS2_PLACEMENT_3D('',#31716,#20240,#20241);
#16822=AXIS2_PLACEMENT_3D('',#31725,#20246,#20247);
#16823=AXIS2_PLACEMENT_3D('',#31731,#20251,#20252);
#16824=AXIS2_PLACEMENT_3D('',#31737,#20256,#20257);
#16825=AXIS2_PLACEMENT_3D('',#31743,#20261,#20262);
#16826=AXIS2_PLACEMENT_3D('',#31749,#20266,#20267);
#16827=AXIS2_PLACEMENT_3D('',#31755,#20271,#20272);
#16828=AXIS2_PLACEMENT_3D('',#31758,#20275,#20276);
#16829=AXIS2_PLACEMENT_3D('',#31759,#20277,#20278);
#16830=AXIS2_PLACEMENT_3D('',#31760,#20279,#20280);
#16831=AXIS2_PLACEMENT_3D('',#31769,#20285,#20286);
#16832=AXIS2_PLACEMENT_3D('',#31775,#20290,#20291);
#16833=AXIS2_PLACEMENT_3D('',#31781,#20295,#20296);
#16834=AXIS2_PLACEMENT_3D('',#31787,#20300,#20301);
#16835=AXIS2_PLACEMENT_3D('',#31793,#20305,#20306);
#16836=AXIS2_PLACEMENT_3D('',#31799,#20310,#20311);
#16837=AXIS2_PLACEMENT_3D('',#31802,#20314,#20315);
#16838=AXIS2_PLACEMENT_3D('',#31803,#20316,#20317);
#16839=AXIS2_PLACEMENT_3D('',#31804,#20318,#20319);
#16840=AXIS2_PLACEMENT_3D('',#31813,#20324,#20325);
#16841=AXIS2_PLACEMENT_3D('',#31819,#20329,#20330);
#16842=AXIS2_PLACEMENT_3D('',#31825,#20334,#20335);
#16843=AXIS2_PLACEMENT_3D('',#31831,#20339,#20340);
#16844=AXIS2_PLACEMENT_3D('',#31837,#20344,#20345);
#16845=AXIS2_PLACEMENT_3D('',#31843,#20349,#20350);
#16846=AXIS2_PLACEMENT_3D('',#31846,#20353,#20354);
#16847=AXIS2_PLACEMENT_3D('',#31847,#20355,#20356);
#16848=AXIS2_PLACEMENT_3D('',#31848,#20357,#20358);
#16849=AXIS2_PLACEMENT_3D('',#31857,#20363,#20364);
#16850=AXIS2_PLACEMENT_3D('',#31863,#20368,#20369);
#16851=AXIS2_PLACEMENT_3D('',#31869,#20373,#20374);
#16852=AXIS2_PLACEMENT_3D('',#31875,#20378,#20379);
#16853=AXIS2_PLACEMENT_3D('',#31881,#20383,#20384);
#16854=AXIS2_PLACEMENT_3D('',#31887,#20388,#20389);
#16855=AXIS2_PLACEMENT_3D('',#31890,#20392,#20393);
#16856=AXIS2_PLACEMENT_3D('',#31891,#20394,#20395);
#16857=AXIS2_PLACEMENT_3D('',#31892,#20396,#20397);
#16858=AXIS2_PLACEMENT_3D('',#31894,#20398,#20399);
#16859=AXIS2_PLACEMENT_3D('',#31897,#20401,#20402);
#16860=AXIS2_PLACEMENT_3D('',#31898,#20403,#20404);
#16861=AXIS2_PLACEMENT_3D('',#31900,#20405,#20406);
#16862=AXIS2_PLACEMENT_3D('',#31903,#20408,#20409);
#16863=AXIS2_PLACEMENT_3D('',#31904,#20410,#20411);
#16864=AXIS2_PLACEMENT_3D('',#31906,#20412,#20413);
#16865=AXIS2_PLACEMENT_3D('',#31909,#20415,#20416);
#16866=AXIS2_PLACEMENT_3D('',#31910,#20417,#20418);
#16867=AXIS2_PLACEMENT_3D('',#31912,#20419,#20420);
#16868=AXIS2_PLACEMENT_3D('',#31915,#20422,#20423);
#16869=AXIS2_PLACEMENT_3D('',#31916,#20424,#20425);
#16870=AXIS2_PLACEMENT_3D('',#31925,#20430,#20431);
#16871=AXIS2_PLACEMENT_3D('',#31934,#20436,#20437);
#16872=AXIS2_PLACEMENT_3D('',#31937,#20440,#20441);
#16873=AXIS2_PLACEMENT_3D('',#31939,#20443,#20444);
#16874=AXIS2_PLACEMENT_3D('',#31941,#20446,#20447);
#16875=AXIS2_PLACEMENT_3D('',#31942,#20448,#20449);
#16876=AXIS2_PLACEMENT_3D('',#31951,#20454,#20455);
#16877=AXIS2_PLACEMENT_3D('',#31957,#20459,#20460);
#16878=AXIS2_PLACEMENT_3D('',#31963,#20464,#20465);
#16879=AXIS2_PLACEMENT_3D('',#31966,#20468,#20469);
#16880=AXIS2_PLACEMENT_3D('',#31967,#20470,#20471);
#16881=AXIS2_PLACEMENT_3D('',#31968,#20472,#20473);
#16882=AXIS2_PLACEMENT_3D('',#31977,#20478,#20479);
#16883=AXIS2_PLACEMENT_3D('',#31983,#20483,#20484);
#16884=AXIS2_PLACEMENT_3D('',#31989,#20488,#20489);
#16885=AXIS2_PLACEMENT_3D('',#31992,#20492,#20493);
#16886=AXIS2_PLACEMENT_3D('',#31993,#20494,#20495);
#16887=AXIS2_PLACEMENT_3D('',#31994,#20496,#20497);
#16888=AXIS2_PLACEMENT_3D('',#32003,#20502,#20503);
#16889=AXIS2_PLACEMENT_3D('',#32009,#20507,#20508);
#16890=AXIS2_PLACEMENT_3D('',#32015,#20512,#20513);
#16891=AXIS2_PLACEMENT_3D('',#32018,#20516,#20517);
#16892=AXIS2_PLACEMENT_3D('',#32019,#20518,#20519);
#16893=AXIS2_PLACEMENT_3D('',#32020,#20520,#20521);
#16894=AXIS2_PLACEMENT_3D('',#32029,#20526,#20527);
#16895=AXIS2_PLACEMENT_3D('',#32035,#20531,#20532);
#16896=AXIS2_PLACEMENT_3D('',#32041,#20536,#20537);
#16897=AXIS2_PLACEMENT_3D('',#32044,#20540,#20541);
#16898=AXIS2_PLACEMENT_3D('',#32045,#20542,#20543);
#16899=AXIS2_PLACEMENT_3D('',#32046,#20544,#20545);
#16900=AXIS2_PLACEMENT_3D('',#32055,#20550,#20551);
#16901=AXIS2_PLACEMENT_3D('',#32061,#20555,#20556);
#16902=AXIS2_PLACEMENT_3D('',#32067,#20560,#20561);
#16903=AXIS2_PLACEMENT_3D('',#32070,#20564,#20565);
#16904=AXIS2_PLACEMENT_3D('',#32071,#20566,#20567);
#16905=AXIS2_PLACEMENT_3D('',#32072,#20568,#20569);
#16906=AXIS2_PLACEMENT_3D('',#32081,#20574,#20575);
#16907=AXIS2_PLACEMENT_3D('',#32087,#20579,#20580);
#16908=AXIS2_PLACEMENT_3D('',#32093,#20584,#20585);
#16909=AXIS2_PLACEMENT_3D('',#32096,#20588,#20589);
#16910=AXIS2_PLACEMENT_3D('',#32097,#20590,#20591);
#16911=AXIS2_PLACEMENT_3D('',#32098,#20592,#20593);
#16912=AXIS2_PLACEMENT_3D('',#32107,#20598,#20599);
#16913=AXIS2_PLACEMENT_3D('',#32113,#20603,#20604);
#16914=AXIS2_PLACEMENT_3D('',#32119,#20608,#20609);
#16915=AXIS2_PLACEMENT_3D('',#32122,#20612,#20613);
#16916=AXIS2_PLACEMENT_3D('',#32123,#20614,#20615);
#16917=AXIS2_PLACEMENT_3D('',#32124,#20616,#20617);
#16918=AXIS2_PLACEMENT_3D('',#32133,#20622,#20623);
#16919=AXIS2_PLACEMENT_3D('',#32139,#20627,#20628);
#16920=AXIS2_PLACEMENT_3D('',#32145,#20632,#20633);
#16921=AXIS2_PLACEMENT_3D('',#32148,#20636,#20637);
#16922=AXIS2_PLACEMENT_3D('',#32149,#20638,#20639);
#16923=AXIS2_PLACEMENT_3D('',#32150,#20640,#20641);
#16924=AXIS2_PLACEMENT_3D('',#32159,#20646,#20647);
#16925=AXIS2_PLACEMENT_3D('',#32165,#20651,#20652);
#16926=AXIS2_PLACEMENT_3D('',#32171,#20656,#20657);
#16927=AXIS2_PLACEMENT_3D('',#32174,#20660,#20661);
#16928=AXIS2_PLACEMENT_3D('',#32175,#20662,#20663);
#16929=AXIS2_PLACEMENT_3D('',#32176,#20664,#20665);
#16930=AXIS2_PLACEMENT_3D('',#32185,#20670,#20671);
#16931=AXIS2_PLACEMENT_3D('',#32191,#20675,#20676);
#16932=AXIS2_PLACEMENT_3D('',#32197,#20680,#20681);
#16933=AXIS2_PLACEMENT_3D('',#32200,#20684,#20685);
#16934=AXIS2_PLACEMENT_3D('',#32201,#20686,#20687);
#16935=AXIS2_PLACEMENT_3D('',#32202,#20688,#20689);
#16936=AXIS2_PLACEMENT_3D('',#32211,#20694,#20695);
#16937=AXIS2_PLACEMENT_3D('',#32217,#20699,#20700);
#16938=AXIS2_PLACEMENT_3D('',#32223,#20704,#20705);
#16939=AXIS2_PLACEMENT_3D('',#32226,#20708,#20709);
#16940=AXIS2_PLACEMENT_3D('',#32227,#20710,#20711);
#16941=AXIS2_PLACEMENT_3D('',#32228,#20712,#20713);
#16942=AXIS2_PLACEMENT_3D('',#32237,#20718,#20719);
#16943=AXIS2_PLACEMENT_3D('',#32243,#20723,#20724);
#16944=AXIS2_PLACEMENT_3D('',#32249,#20728,#20729);
#16945=AXIS2_PLACEMENT_3D('',#32252,#20732,#20733);
#16946=AXIS2_PLACEMENT_3D('',#32253,#20734,#20735);
#16947=AXIS2_PLACEMENT_3D('',#32254,#20736,#20737);
#16948=AXIS2_PLACEMENT_3D('',#32263,#20742,#20743);
#16949=AXIS2_PLACEMENT_3D('',#32269,#20747,#20748);
#16950=AXIS2_PLACEMENT_3D('',#32275,#20752,#20753);
#16951=AXIS2_PLACEMENT_3D('',#32278,#20756,#20757);
#16952=AXIS2_PLACEMENT_3D('',#32279,#20758,#20759);
#16953=AXIS2_PLACEMENT_3D('',#32280,#20760,#20761);
#16954=AXIS2_PLACEMENT_3D('',#32289,#20766,#20767);
#16955=AXIS2_PLACEMENT_3D('',#32295,#20771,#20772);
#16956=AXIS2_PLACEMENT_3D('',#32301,#20776,#20777);
#16957=AXIS2_PLACEMENT_3D('',#32304,#20780,#20781);
#16958=AXIS2_PLACEMENT_3D('',#32305,#20782,#20783);
#16959=AXIS2_PLACEMENT_3D('',#32306,#20784,#20785);
#16960=AXIS2_PLACEMENT_3D('',#32315,#20790,#20791);
#16961=AXIS2_PLACEMENT_3D('',#32321,#20795,#20796);
#16962=AXIS2_PLACEMENT_3D('',#32327,#20800,#20801);
#16963=AXIS2_PLACEMENT_3D('',#32330,#20804,#20805);
#16964=AXIS2_PLACEMENT_3D('',#32331,#20806,#20807);
#16965=AXIS2_PLACEMENT_3D('',#32332,#20808,#20809);
#16966=AXIS2_PLACEMENT_3D('',#32341,#20814,#20815);
#16967=AXIS2_PLACEMENT_3D('',#32347,#20819,#20820);
#16968=AXIS2_PLACEMENT_3D('',#32353,#20824,#20825);
#16969=AXIS2_PLACEMENT_3D('',#32356,#20828,#20829);
#16970=AXIS2_PLACEMENT_3D('',#32357,#20830,#20831);
#16971=AXIS2_PLACEMENT_3D('',#32358,#20832,#20833);
#16972=AXIS2_PLACEMENT_3D('',#32367,#20838,#20839);
#16973=AXIS2_PLACEMENT_3D('',#32373,#20843,#20844);
#16974=AXIS2_PLACEMENT_3D('',#32379,#20848,#20849);
#16975=AXIS2_PLACEMENT_3D('',#32382,#20852,#20853);
#16976=AXIS2_PLACEMENT_3D('',#32383,#20854,#20855);
#16977=AXIS2_PLACEMENT_3D('',#32384,#20856,#20857);
#16978=AXIS2_PLACEMENT_3D('',#32393,#20862,#20863);
#16979=AXIS2_PLACEMENT_3D('',#32399,#20867,#20868);
#16980=AXIS2_PLACEMENT_3D('',#32405,#20872,#20873);
#16981=AXIS2_PLACEMENT_3D('',#32408,#20876,#20877);
#16982=AXIS2_PLACEMENT_3D('',#32409,#20878,#20879);
#16983=AXIS2_PLACEMENT_3D('',#32410,#20880,#20881);
#16984=AXIS2_PLACEMENT_3D('',#32419,#20886,#20887);
#16985=AXIS2_PLACEMENT_3D('',#32425,#20891,#20892);
#16986=AXIS2_PLACEMENT_3D('',#32431,#20896,#20897);
#16987=AXIS2_PLACEMENT_3D('',#32434,#20900,#20901);
#16988=AXIS2_PLACEMENT_3D('',#32435,#20902,#20903);
#16989=AXIS2_PLACEMENT_3D('',#32436,#20904,#20905);
#16990=AXIS2_PLACEMENT_3D('',#32445,#20910,#20911);
#16991=AXIS2_PLACEMENT_3D('',#32451,#20915,#20916);
#16992=AXIS2_PLACEMENT_3D('',#32457,#20920,#20921);
#16993=AXIS2_PLACEMENT_3D('',#32460,#20924,#20925);
#16994=AXIS2_PLACEMENT_3D('',#32461,#20926,#20927);
#16995=AXIS2_PLACEMENT_3D('',#32462,#20928,#20929);
#16996=AXIS2_PLACEMENT_3D('',#32471,#20934,#20935);
#16997=AXIS2_PLACEMENT_3D('',#32477,#20939,#20940);
#16998=AXIS2_PLACEMENT_3D('',#32483,#20944,#20945);
#16999=AXIS2_PLACEMENT_3D('',#32486,#20948,#20949);
#17000=AXIS2_PLACEMENT_3D('',#32487,#20950,#20951);
#17001=AXIS2_PLACEMENT_3D('',#32488,#20952,#20953);
#17002=AXIS2_PLACEMENT_3D('',#32497,#20958,#20959);
#17003=AXIS2_PLACEMENT_3D('',#32503,#20963,#20964);
#17004=AXIS2_PLACEMENT_3D('',#32509,#20968,#20969);
#17005=AXIS2_PLACEMENT_3D('',#32512,#20972,#20973);
#17006=AXIS2_PLACEMENT_3D('',#32513,#20974,#20975);
#17007=AXIS2_PLACEMENT_3D('',#32514,#20976,#20977);
#17008=AXIS2_PLACEMENT_3D('',#32515,#20978,#20979);
#17009=AXIS2_PLACEMENT_3D('',#32518,#20980,#20981);
#17010=AXIS2_PLACEMENT_3D('',#32519,#20982,#20983);
#17011=AXIS2_PLACEMENT_3D('',#32521,#20984,#20985);
#17012=AXIS2_PLACEMENT_3D('',#32522,#20986,#20987);
#17013=AXIS2_PLACEMENT_3D('',#32523,#20988,#20989);
#17014=AXIS2_PLACEMENT_3D('',#32526,#20990,#20991);
#17015=AXIS2_PLACEMENT_3D('',#32528,#20992,#20993);
#17016=AXIS2_PLACEMENT_3D('',#32530,#20994,#20995);
#17017=AXIS2_PLACEMENT_3D('',#32533,#20997,#20998);
#17018=AXIS2_PLACEMENT_3D('',#32535,#20999,#21000);
#17019=AXIS2_PLACEMENT_3D('',#32537,#21001,#21002);
#17020=AXIS2_PLACEMENT_3D('',#32538,#21003,#21004);
#17021=AXIS2_PLACEMENT_3D('',#32539,#21005,#21006);
#17022=AXIS2_PLACEMENT_3D('',#32541,#21007,#21008);
#17023=AXIS2_PLACEMENT_3D('',#32544,#21010,#21011);
#17024=AXIS2_PLACEMENT_3D('',#32545,#21012,#21013);
#17025=AXIS2_PLACEMENT_3D('',#32547,#21015,#21016);
#17026=AXIS2_PLACEMENT_3D('',#32548,#21017,#21018);
#17027=AXIS2_PLACEMENT_3D('',#32549,#21019,#21020);
#17028=AXIS2_PLACEMENT_3D('',#32553,#21023,#21024);
#17029=AXIS2_PLACEMENT_3D('',#32557,#21027,#21028);
#17030=AXIS2_PLACEMENT_3D('',#32561,#21031,#21032);
#17031=AXIS2_PLACEMENT_3D('',#32565,#21035,#21036);
#17032=AXIS2_PLACEMENT_3D('',#32569,#21039,#21040);
#17033=AXIS2_PLACEMENT_3D('',#32573,#21043,#21044);
#17034=AXIS2_PLACEMENT_3D('',#32576,#21045,#21046);
#17035=AXIS2_PLACEMENT_3D('',#32578,#21047,#21048);
#17036=AXIS2_PLACEMENT_3D('',#32580,#21049,#21050);
#17037=AXIS2_PLACEMENT_3D('',#32582,#21051,#21052);
#17038=AXIS2_PLACEMENT_3D('',#32584,#21053,#21054);
#17039=AXIS2_PLACEMENT_3D('',#32585,#21055,#21056);
#17040=AXIS2_PLACEMENT_3D('',#32586,#21057,#21058);
#17041=AXIS2_PLACEMENT_3D('',#32594,#21059,#21060);
#17042=AXIS2_PLACEMENT_3D('',#32602,#21061,#21062);
#17043=AXIS2_PLACEMENT_3D('',#32610,#21063,#21064);
#17044=AXIS2_PLACEMENT_3D('',#32618,#21065,#21066);
#17045=AXIS2_PLACEMENT_3D('',#32626,#21067,#21068);
#17046=AXIS2_PLACEMENT_3D('',#32634,#21069,#21070);
#17047=AXIS2_PLACEMENT_3D('',#32637,#21073,#21074);
#17048=AXIS2_PLACEMENT_3D('',#32639,#21076,#21077);
#17049=AXIS2_PLACEMENT_3D('',#32641,#21079,#21080);
#17050=AXIS2_PLACEMENT_3D('',#32643,#21082,#21083);
#17051=AXIS2_PLACEMENT_3D('',#32645,#21085,#21086);
#17052=AXIS2_PLACEMENT_3D('',#32646,#21087,#21088);
#17053=AXIS2_PLACEMENT_3D('',#32647,#21089,#21090);
#17054=AXIS2_PLACEMENT_3D('',#32649,#21091,#21092);
#17055=AXIS2_PLACEMENT_3D('',#32652,#21094,#21095);
#17056=AXIS2_PLACEMENT_3D('',#32653,#21096,#21097);
#17057=AXIS2_PLACEMENT_3D('',#32655,#21098,#21099);
#17058=AXIS2_PLACEMENT_3D('',#32658,#21101,#21102);
#17059=AXIS2_PLACEMENT_3D('',#32659,#21103,#21104);
#17060=AXIS2_PLACEMENT_3D('',#32660,#21105,#21106);
#17061=AXIS2_PLACEMENT_3D('',#32661,#21107,#21108);
#17062=AXIS2_PLACEMENT_3D('',#32662,#21109,#21110);
#17063=AXIS2_PLACEMENT_3D('',#32664,#21111,#21112);
#17064=AXIS2_PLACEMENT_3D('',#32668,#21114,#21115);
#17065=AXIS2_PLACEMENT_3D('',#32669,#21116,#21117);
#17066=AXIS2_PLACEMENT_3D('',#32670,#21118,#21119);
#17067=AXIS2_PLACEMENT_3D('',#32673,#21120,#21121);
#17068=AXIS2_PLACEMENT_3D('',#32675,#21123,#21124);
#17069=AXIS2_PLACEMENT_3D('',#32676,#21125,#21126);
#17070=AXIS2_PLACEMENT_3D('',#32678,#21127,#21128);
#17071=AXIS2_PLACEMENT_3D('',#32681,#21130,#21131);
#17072=AXIS2_PLACEMENT_3D('',#32682,#21132,#21133);
#17073=AXIS2_PLACEMENT_3D('',#32684,#21135,#21136);
#17074=AXIS2_PLACEMENT_3D('',#32705,#21139,#21140);
#17075=AXIS2_PLACEMENT_3D('',#32723,#21142,#21143);
#17076=AXIS2_PLACEMENT_3D('',#32741,#21145,#21146);
#17077=AXIS2_PLACEMENT_3D('',#32759,#21148,#21149);
#17078=AXIS2_PLACEMENT_3D('',#32777,#21151,#21152);
#17079=AXIS2_PLACEMENT_3D('',#32792,#21153,#21154);
#17080=AXIS2_PLACEMENT_3D('',#32793,#21155,#21156);
#17081=AXIS2_PLACEMENT_3D('',#32794,#21157,#21158);
#17082=AXIS2_PLACEMENT_3D('',#32795,#21159,#21160);
#17083=AXIS2_PLACEMENT_3D('',#32796,#21161,#21162);
#17084=AXIS2_PLACEMENT_3D('',#32797,#21163,#21164);
#17085=AXIS2_PLACEMENT_3D('',#32798,#21165,#21166);
#17086=AXIS2_PLACEMENT_3D('',#32799,#21167,#21168);
#17087=AXIS2_PLACEMENT_3D('',#32800,#21169,#21170);
#17088=AXIS2_PLACEMENT_3D('',#32801,#21171,#21172);
#17089=AXIS2_PLACEMENT_3D('',#32802,#21173,#21174);
#17090=AXIS2_PLACEMENT_3D('',#32803,#21175,#21176);
#17091=AXIS2_PLACEMENT_3D('',#32804,#21177,#21178);
#17092=AXIS2_PLACEMENT_3D('',#32805,#21179,#21180);
#17093=AXIS2_PLACEMENT_3D('',#32806,#21181,#21182);
#17094=AXIS2_PLACEMENT_3D('',#32807,#21183,#21184);
#17095=AXIS2_PLACEMENT_3D('',#32808,#21185,#21186);
#17096=AXIS2_PLACEMENT_3D('',#32809,#21187,#21188);
#17097=AXIS2_PLACEMENT_3D('',#32810,#21189,#21190);
#17098=AXIS2_PLACEMENT_3D('',#32811,#21191,#21192);
#17099=AXIS2_PLACEMENT_3D('',#32812,#21193,#21194);
#17100=AXIS2_PLACEMENT_3D('',#32813,#21195,#21196);
#17101=AXIS2_PLACEMENT_3D('',#32814,#21197,#21198);
#17102=AXIS2_PLACEMENT_3D('',#32815,#21199,#21200);
#17103=AXIS2_PLACEMENT_3D('',#32816,#21201,#21202);
#17104=AXIS2_PLACEMENT_3D('',#32817,#21203,#21204);
#17105=AXIS2_PLACEMENT_3D('',#32818,#21205,#21206);
#17106=AXIS2_PLACEMENT_3D('',#32819,#21207,#21208);
#17107=AXIS2_PLACEMENT_3D('',#32820,#21209,#21210);
#17108=AXIS2_PLACEMENT_3D('',#32821,#21211,#21212);
#17109=AXIS2_PLACEMENT_3D('',#32822,#21213,#21214);
#17110=AXIS2_PLACEMENT_3D('',#32823,#21215,#21216);
#17111=AXIS2_PLACEMENT_3D('',#32824,#21217,#21218);
#17112=AXIS2_PLACEMENT_3D('',#32825,#21219,#21220);
#17113=AXIS2_PLACEMENT_3D('',#32826,#21221,#21222);
#17114=AXIS2_PLACEMENT_3D('',#32827,#21223,#21224);
#17115=AXIS2_PLACEMENT_3D('',#32828,#21225,#21226);
#17116=AXIS2_PLACEMENT_3D('',#32829,#21227,#21228);
#17117=AXIS2_PLACEMENT_3D('',#32830,#21229,#21230);
#17118=AXIS2_PLACEMENT_3D('',#32831,#21231,#21232);
#17119=AXIS2_PLACEMENT_3D('',#32832,#21233,#21234);
#17120=AXIS2_PLACEMENT_3D('',#32833,#21235,#21236);
#17121=AXIS2_PLACEMENT_3D('',#32834,#21237,#21238);
#17122=AXIS2_PLACEMENT_3D('',#32835,#21239,#21240);
#17123=AXIS2_PLACEMENT_3D('',#32836,#21241,#21242);
#17124=AXIS2_PLACEMENT_3D('',#32837,#21243,#21244);
#17125=AXIS2_PLACEMENT_3D('',#32838,#21245,#21246);
#17126=AXIS2_PLACEMENT_3D('',#32839,#21247,#21248);
#17127=AXIS2_PLACEMENT_3D('',#32840,#21249,#21250);
#17128=AXIS2_PLACEMENT_3D('',#32841,#21251,#21252);
#17129=AXIS2_PLACEMENT_3D('',#32842,#21253,#21254);
#17130=AXIS2_PLACEMENT_3D('',#32843,#21255,#21256);
#17131=AXIS2_PLACEMENT_3D('',#32844,#21257,#21258);
#17132=AXIS2_PLACEMENT_3D('',#32845,#21259,#21260);
#17133=AXIS2_PLACEMENT_3D('',#32846,#21261,#21262);
#17134=AXIS2_PLACEMENT_3D('',#32847,#21263,#21264);
#17135=AXIS2_PLACEMENT_3D('',#32848,#21265,#21266);
#17136=AXIS2_PLACEMENT_3D('',#32849,#21267,#21268);
#17137=AXIS2_PLACEMENT_3D('',#32850,#21269,#21270);
#17138=AXIS2_PLACEMENT_3D('',#32851,#21271,#21272);
#17139=AXIS2_PLACEMENT_3D('',#32852,#21273,#21274);
#17140=AXIS2_PLACEMENT_3D('',#32853,#21275,#21276);
#17141=AXIS2_PLACEMENT_3D('',#32854,#21277,#21278);
#17142=AXIS2_PLACEMENT_3D('',#32855,#21279,#21280);
#17143=AXIS2_PLACEMENT_3D('',#32856,#21281,#21282);
#17144=AXIS2_PLACEMENT_3D('',#32857,#21283,#21284);
#17145=AXIS2_PLACEMENT_3D('',#32858,#21285,#21286);
#17146=AXIS2_PLACEMENT_3D('',#32859,#21287,#21288);
#17147=AXIS2_PLACEMENT_3D('',#32860,#21289,#21290);
#17148=AXIS2_PLACEMENT_3D('',#32861,#21291,#21292);
#17149=AXIS2_PLACEMENT_3D('',#32862,#21293,#21294);
#17150=AXIS2_PLACEMENT_3D('',#32863,#21295,#21296);
#17151=AXIS2_PLACEMENT_3D('',#32864,#21297,#21298);
#17152=AXIS2_PLACEMENT_3D('',#32865,#21299,#21300);
#17153=AXIS2_PLACEMENT_3D('',#32866,#21301,#21302);
#17154=AXIS2_PLACEMENT_3D('',#32867,#21303,#21304);
#17155=AXIS2_PLACEMENT_3D('',#32868,#21305,#21306);
#17156=AXIS2_PLACEMENT_3D('',#32869,#21307,#21308);
#17157=DIRECTION('axis',(0.,0.,1.));
#17158=DIRECTION('refdir',(1.,0.,0.));
#17159=DIRECTION('axis',(0.,0.,1.));
#17160=DIRECTION('refdir',(1.,0.,0.));
#17161=DIRECTION('center_axis',(1.,0.,0.));
#17162=DIRECTION('ref_axis',(0.,0.,-1.));
#17163=DIRECTION('',(0.,1.,0.));
#17164=DIRECTION('',(0.,0.,1.));
#17165=DIRECTION('',(0.,1.,0.));
#17166=DIRECTION('',(0.,0.,1.));
#17167=DIRECTION('center_axis',(0.,-1.,0.));
#17168=DIRECTION('ref_axis',(0.,0.,-1.));
#17169=DIRECTION('',(1.,0.,0.));
#17170=DIRECTION('',(0.,0.,1.));
#17171=DIRECTION('',(1.,0.,0.));
#17172=DIRECTION('center_axis',(-1.,0.,0.));
#17173=DIRECTION('ref_axis',(0.,0.,1.));
#17174=DIRECTION('',(0.,-1.,0.));
#17175=DIRECTION('',(0.,0.,1.));
#17176=DIRECTION('',(0.,-1.,0.));
#17177=DIRECTION('center_axis',(0.,1.,0.));
#17178=DIRECTION('ref_axis',(0.,0.,1.));
#17179=DIRECTION('',(-1.,0.,0.));
#17180=DIRECTION('',(-1.,0.,0.));
#17181=DIRECTION('center_axis',(0.,0.,-1.));
#17182=DIRECTION('ref_axis',(-1.,0.,0.));
#17183=DIRECTION('',(0.,1.,0.));
#17184=DIRECTION('',(-1.,0.,0.));
#17185=DIRECTION('',(0.,-1.,0.));
#17186=DIRECTION('',(1.,0.,0.));
#17187=DIRECTION('center_axis',(0.,0.,-1.));
#17188=DIRECTION('ref_axis',(-1.,0.,0.));
#17189=DIRECTION('',(-1.,0.,0.));
#17190=DIRECTION('',(0.,1.,0.));
#17191=DIRECTION('',(1.,0.,0.));
#17192=DIRECTION('',(0.,-1.,0.));
#17193=DIRECTION('center_axis',(1.,0.,0.));
#17194=DIRECTION('ref_axis',(0.,0.,-1.));
#17195=DIRECTION('',(0.,0.,1.));
#17196=DIRECTION('',(0.,0.,1.));
#17197=DIRECTION('center_axis',(0.,-1.,0.));
#17198=DIRECTION('ref_axis',(0.,0.,-1.));
#17199=DIRECTION('',(0.,0.,1.));
#17200=DIRECTION('center_axis',(-1.,0.,0.));
#17201=DIRECTION('ref_axis',(0.,0.,1.));
#17202=DIRECTION('',(0.,0.,1.));
#17203=DIRECTION('center_axis',(0.,1.,0.));
#17204=DIRECTION('ref_axis',(0.,0.,1.));
#17205=DIRECTION('center_axis',(0.,0.,-1.));
#17206=DIRECTION('ref_axis',(-1.,0.,0.));
#17207=DIRECTION('',(0.,-1.,0.));
#17208=DIRECTION('',(-1.,0.,0.));
#17209=DIRECTION('',(0.,-1.,0.));
#17210=DIRECTION('',(-1.,0.,0.));
#17211=DIRECTION('center_axis',(0.,1.,9.62873847203288E-17));
#17212=DIRECTION('ref_axis',(0.,-9.62873847203288E-17,1.));
#17213=DIRECTION('',(0.,9.62873847203288E-17,-1.));
#17214=DIRECTION('',(-1.,0.,0.));
#17215=DIRECTION('',(0.,9.62873847203288E-17,-1.));
#17216=DIRECTION('center_axis',(-1.,0.,0.));
#17217=DIRECTION('ref_axis',(0.,0.,1.));
#17218=DIRECTION('center_axis',(-1.,0.,0.));
#17219=DIRECTION('ref_axis',(0.,0.,-1.));
#17220=DIRECTION('',(-1.,0.,0.));
#17221=DIRECTION('center_axis',(-1.,0.,0.));
#17222=DIRECTION('ref_axis',(0.,0.,-1.));
#17223=DIRECTION('center_axis',(0.,1.,7.93016446160826E-17));
#17224=DIRECTION('ref_axis',(0.,-7.93016446160826E-17,1.));
#17225=DIRECTION('',(0.,7.93016446160826E-17,-1.));
#17226=DIRECTION('',(-1.,0.,0.));
#17227=DIRECTION('',(0.,7.93016446160826E-17,-1.));
#17228=DIRECTION('center_axis',(0.,0.,1.));
#17229=DIRECTION('ref_axis',(1.,0.,0.));
#17230=DIRECTION('',(0.,1.,0.));
#17231=DIRECTION('',(-1.,0.,0.));
#17232=DIRECTION('',(0.,1.,0.));
#17233=DIRECTION('center_axis',(0.,-1.,0.));
#17234=DIRECTION('ref_axis',(0.,0.,-1.));
#17235=DIRECTION('',(0.,0.,1.));
#17236=DIRECTION('',(0.,0.,1.));
#17237=DIRECTION('center_axis',(1.,0.,0.));
#17238=DIRECTION('ref_axis',(0.,0.,-1.));
#17239=DIRECTION('center_axis',(1.,0.,0.));
#17240=DIRECTION('ref_axis',(0.,0.,-1.));
#17241=DIRECTION('center_axis',(0.,0.,-1.));
#17242=DIRECTION('ref_axis',(1.,0.,0.));
#17243=DIRECTION('',(0.,-1.,0.));
#17244=DIRECTION('',(1.,0.,0.));
#17245=DIRECTION('',(0.,-1.,0.));
#17246=DIRECTION('',(1.,0.,0.));
#17247=DIRECTION('center_axis',(0.,1.,9.62873847203288E-17));
#17248=DIRECTION('ref_axis',(0.,-9.62873847203288E-17,1.));
#17249=DIRECTION('',(0.,9.62873847203288E-17,-1.));
#17250=DIRECTION('',(0.,9.62873847203288E-17,-1.));
#17251=DIRECTION('',(1.,0.,0.));
#17252=DIRECTION('center_axis',(1.,0.,0.));
#17253=DIRECTION('ref_axis',(0.,0.,1.));
#17254=DIRECTION('center_axis',(-1.,0.,0.));
#17255=DIRECTION('ref_axis',(0.,0.,-1.));
#17256=DIRECTION('center_axis',(-1.,0.,0.));
#17257=DIRECTION('ref_axis',(0.,0.,-1.));
#17258=DIRECTION('',(1.,0.,0.));
#17259=DIRECTION('center_axis',(0.,1.,7.93016446160826E-17));
#17260=DIRECTION('ref_axis',(0.,-7.93016446160826E-17,1.));
#17261=DIRECTION('',(0.,7.93016446160826E-17,-1.));
#17262=DIRECTION('',(0.,7.93016446160826E-17,-1.));
#17263=DIRECTION('',(1.,0.,0.));
#17264=DIRECTION('center_axis',(0.,0.,1.));
#17265=DIRECTION('ref_axis',(-1.,0.,0.));
#17266=DIRECTION('',(0.,1.,0.));
#17267=DIRECTION('',(0.,1.,0.));
#17268=DIRECTION('',(1.,0.,0.));
#17269=DIRECTION('center_axis',(0.,-1.,0.));
#17270=DIRECTION('ref_axis',(0.,0.,-1.));
#17271=DIRECTION('',(0.,0.,1.));
#17272=DIRECTION('',(0.,0.,1.));
#17273=DIRECTION('center_axis',(-1.,0.,0.));
#17274=DIRECTION('ref_axis',(0.,0.,-1.));
#17275=DIRECTION('center_axis',(-1.,0.,0.));
#17276=DIRECTION('ref_axis',(0.,0.,-1.));
#17277=DIRECTION('center_axis',(0.,-1.,0.));
#17278=DIRECTION('ref_axis',(0.,0.,-1.));
#17279=DIRECTION('center_axis',(0.,1.,0.));
#17280=DIRECTION('ref_axis',(0.,0.,1.));
#17281=DIRECTION('',(0.,-1.,0.));
#17282=DIRECTION('center_axis',(0.,1.,0.));
#17283=DIRECTION('ref_axis',(0.,0.,1.));
#17284=DIRECTION('center_axis',(0.,-1.,0.));
#17285=DIRECTION('ref_axis',(0.,0.,-1.));
#17286=DIRECTION('center_axis',(0.,1.,0.));
#17287=DIRECTION('ref_axis',(0.,0.,1.));
#17288=DIRECTION('',(0.,-1.,0.));
#17289=DIRECTION('center_axis',(0.,1.,0.));
#17290=DIRECTION('ref_axis',(0.,0.,1.));
#17291=DIRECTION('center_axis',(0.,-1.,0.));
#17292=DIRECTION('ref_axis',(0.,0.,-1.));
#17293=DIRECTION('center_axis',(0.,1.,0.));
#17294=DIRECTION('ref_axis',(0.,0.,1.));
#17295=DIRECTION('',(0.,-1.,0.));
#17296=DIRECTION('center_axis',(0.,1.,0.));
#17297=DIRECTION('ref_axis',(0.,0.,1.));
#17298=DIRECTION('center_axis',(0.,-1.,0.));
#17299=DIRECTION('ref_axis',(0.,0.,-1.));
#17300=DIRECTION('center_axis',(0.,1.,0.));
#17301=DIRECTION('ref_axis',(0.,0.,1.));
#17302=DIRECTION('',(0.,-1.,0.));
#17303=DIRECTION('center_axis',(0.,1.,0.));
#17304=DIRECTION('ref_axis',(0.,0.,1.));
#17305=DIRECTION('center_axis',(0.,-1.,0.));
#17306=DIRECTION('ref_axis',(0.,0.,-1.));
#17307=DIRECTION('center_axis',(0.,1.,0.));
#17308=DIRECTION('ref_axis',(0.,0.,1.));
#17309=DIRECTION('',(0.,-1.,0.));
#17310=DIRECTION('center_axis',(0.,1.,0.));
#17311=DIRECTION('ref_axis',(0.,0.,1.));
#17312=DIRECTION('center_axis',(0.,-1.,0.));
#17313=DIRECTION('ref_axis',(0.,0.,-1.));
#17314=DIRECTION('center_axis',(0.,1.,0.));
#17315=DIRECTION('ref_axis',(0.,0.,1.));
#17316=DIRECTION('',(0.,-1.,0.));
#17317=DIRECTION('center_axis',(0.,1.,0.));
#17318=DIRECTION('ref_axis',(0.,0.,1.));
#17319=DIRECTION('center_axis',(0.,1.,0.));
#17320=DIRECTION('ref_axis',(0.,0.,1.));
#17321=DIRECTION('',(0.,0.,1.));
#17322=DIRECTION('',(1.,0.,-1.87133061054672E-16));
#17323=DIRECTION('',(0.,0.,-1.));
#17324=DIRECTION('',(-1.,0.,1.83697019872103E-16));
#17325=DIRECTION('center_axis',(0.,1.,0.));
#17326=DIRECTION('ref_axis',(0.,0.,1.));
#17327=DIRECTION('',(0.,0.,1.));
#17328=DIRECTION('',(-1.,0.,1.83697019872103E-16));
#17329=DIRECTION('',(0.,0.,-1.));
#17330=DIRECTION('',(1.,0.,-1.87133061054672E-16));
#17331=DIRECTION('center_axis',(1.,0.,0.));
#17332=DIRECTION('ref_axis',(0.,0.,-1.));
#17333=DIRECTION('',(0.,-1.,0.));
#17334=DIRECTION('',(0.,-1.,0.));
#17335=DIRECTION('center_axis',(-1.87133061054672E-16,0.,-1.));
#17336=DIRECTION('ref_axis',(-1.,0.,1.87133061054672E-16));
#17337=DIRECTION('',(0.,-1.,0.));
#17338=DIRECTION('center_axis',(-1.,0.,0.));
#17339=DIRECTION('ref_axis',(0.,0.,1.));
#17340=DIRECTION('',(0.,-1.,0.));
#17341=DIRECTION('center_axis',(1.83697019872103E-16,0.,1.));
#17342=DIRECTION('ref_axis',(1.,0.,-1.83697019872103E-16));
#17343=DIRECTION('center_axis',(0.,1.,0.));
#17344=DIRECTION('ref_axis',(0.,0.,1.));
#17345=DIRECTION('center_axis',(0.,1.,0.));
#17346=DIRECTION('ref_axis',(0.,0.,1.));
#17347=DIRECTION('',(0.,1.,0.));
#17348=DIRECTION('center_axis',(0.,1.,0.));
#17349=DIRECTION('ref_axis',(0.,0.,1.));
#17350=DIRECTION('center_axis',(0.,1.,0.));
#17351=DIRECTION('ref_axis',(0.,0.,1.));
#17352=DIRECTION('center_axis',(0.,1.,0.));
#17353=DIRECTION('ref_axis',(0.,0.,1.));
#17354=DIRECTION('',(0.,1.,0.));
#17355=DIRECTION('center_axis',(0.,1.,0.));
#17356=DIRECTION('ref_axis',(0.,0.,1.));
#17357=DIRECTION('center_axis',(0.,1.,0.));
#17358=DIRECTION('ref_axis',(0.,0.,1.));
#17359=DIRECTION('center_axis',(0.,1.,0.));
#17360=DIRECTION('ref_axis',(0.,0.,1.));
#17361=DIRECTION('',(0.,1.,0.));
#17362=DIRECTION('center_axis',(0.,1.,0.));
#17363=DIRECTION('ref_axis',(0.,0.,1.));
#17364=DIRECTION('center_axis',(0.,1.,0.));
#17365=DIRECTION('ref_axis',(0.,0.,1.));
#17366=DIRECTION('center_axis',(0.,1.,0.));
#17367=DIRECTION('ref_axis',(0.,0.,1.));
#17368=DIRECTION('',(0.,1.,0.));
#17369=DIRECTION('center_axis',(0.,1.,0.));
#17370=DIRECTION('ref_axis',(0.,0.,1.));
#17371=DIRECTION('center_axis',(0.,1.,0.));
#17372=DIRECTION('ref_axis',(0.,0.,1.));
#17373=DIRECTION('center_axis',(0.,1.,0.));
#17374=DIRECTION('ref_axis',(0.,0.,1.));
#17375=DIRECTION('',(0.,1.,0.));
#17376=DIRECTION('center_axis',(0.,1.,0.));
#17377=DIRECTION('ref_axis',(0.,0.,1.));
#17378=DIRECTION('center_axis',(-1.,0.,0.));
#17379=DIRECTION('ref_axis',(0.,0.,1.));
#17380=DIRECTION('',(0.,0.,1.));
#17381=DIRECTION('',(0.,1.,0.));
#17382=DIRECTION('',(0.,0.,1.));
#17383=DIRECTION('',(0.,1.,0.));
#17384=DIRECTION('center_axis',(0.,0.,-1.));
#17385=DIRECTION('ref_axis',(-1.,0.,0.));
#17386=DIRECTION('',(-1.,0.,0.));
#17387=DIRECTION('',(0.,1.,0.));
#17388=DIRECTION('',(-1.,0.,0.));
#17389=DIRECTION('center_axis',(1.,0.,0.));
#17390=DIRECTION('ref_axis',(0.,0.,-1.));
#17391=DIRECTION('',(0.,0.,-1.));
#17392=DIRECTION('',(0.,1.,0.));
#17393=DIRECTION('',(0.,0.,-1.));
#17394=DIRECTION('center_axis',(0.,0.,1.));
#17395=DIRECTION('ref_axis',(1.,0.,0.));
#17396=DIRECTION('',(1.,0.,0.));
#17397=DIRECTION('',(1.,0.,0.));
#17398=DIRECTION('center_axis',(0.,-1.,0.));
#17399=DIRECTION('ref_axis',(0.,0.,-1.));
#17400=DIRECTION('center_axis',(0.,-1.,0.));
#17401=DIRECTION('ref_axis',(0.,0.,-1.));
#17402=DIRECTION('center_axis',(0.,1.,0.));
#17403=DIRECTION('ref_axis',(0.,0.,1.));
#17404=DIRECTION('center_axis',(0.,-1.,0.));
#17405=DIRECTION('ref_axis',(0.,0.,1.));
#17406=DIRECTION('',(0.,1.,0.));
#17407=DIRECTION('center_axis',(0.,-1.,0.));
#17408=DIRECTION('ref_axis',(0.,0.,1.));
#17409=DIRECTION('center_axis',(0.,1.,0.));
#17410=DIRECTION('ref_axis',(0.,0.,1.));
#17411=DIRECTION('center_axis',(0.,-1.,0.));
#17412=DIRECTION('ref_axis',(0.,0.,1.));
#17413=DIRECTION('',(0.,1.,0.));
#17414=DIRECTION('center_axis',(0.,-1.,0.));
#17415=DIRECTION('ref_axis',(0.,0.,1.));
#17416=DIRECTION('center_axis',(0.,1.,0.));
#17417=DIRECTION('ref_axis',(0.,0.,1.));
#17418=DIRECTION('center_axis',(0.,-1.,0.));
#17419=DIRECTION('ref_axis',(0.,0.,1.));
#17420=DIRECTION('',(0.,1.,0.));
#17421=DIRECTION('center_axis',(0.,-1.,0.));
#17422=DIRECTION('ref_axis',(0.,0.,1.));
#17423=DIRECTION('center_axis',(0.,1.,0.));
#17424=DIRECTION('ref_axis',(0.,0.,1.));
#17425=DIRECTION('center_axis',(0.,-1.,0.));
#17426=DIRECTION('ref_axis',(0.,0.,1.));
#17427=DIRECTION('',(0.,1.,0.));
#17428=DIRECTION('center_axis',(0.,-1.,0.));
#17429=DIRECTION('ref_axis',(0.,0.,1.));
#17430=DIRECTION('center_axis',(0.,1.,0.));
#17431=DIRECTION('ref_axis',(0.,0.,1.));
#17432=DIRECTION('center_axis',(0.,-1.,0.));
#17433=DIRECTION('ref_axis',(0.,0.,1.));
#17434=DIRECTION('',(0.,1.,0.));
#17435=DIRECTION('center_axis',(0.,-1.,0.));
#17436=DIRECTION('ref_axis',(0.,0.,1.));
#17437=DIRECTION('center_axis',(1.,0.,0.));
#17438=DIRECTION('ref_axis',(0.,0.,1.));
#17439=DIRECTION('',(0.,0.,1.));
#17440=DIRECTION('',(0.,1.,0.));
#17441=DIRECTION('',(0.,0.,1.));
#17442=DIRECTION('',(0.,1.,0.));
#17443=DIRECTION('center_axis',(0.,0.,-1.));
#17444=DIRECTION('ref_axis',(1.,0.,0.));
#17445=DIRECTION('',(1.,0.,0.));
#17446=DIRECTION('',(1.,0.,0.));
#17447=DIRECTION('',(0.,1.,0.));
#17448=DIRECTION('center_axis',(-1.,0.,0.));
#17449=DIRECTION('ref_axis',(0.,0.,-1.));
#17450=DIRECTION('',(0.,0.,-1.));
#17451=DIRECTION('',(0.,0.,-1.));
#17452=DIRECTION('',(0.,1.,0.));
#17453=DIRECTION('center_axis',(0.,0.,1.));
#17454=DIRECTION('ref_axis',(-1.,0.,0.));
#17455=DIRECTION('',(-1.,0.,0.));
#17456=DIRECTION('',(-1.,0.,0.));
#17457=DIRECTION('center_axis',(0.,-1.,0.));
#17458=DIRECTION('ref_axis',(0.,0.,-1.));
#17459=DIRECTION('center_axis',(0.,-1.,0.));
#17460=DIRECTION('ref_axis',(0.,0.,-1.));
#17461=DIRECTION('center_axis',(-1.87133061054672E-16,0.,-1.));
#17462=DIRECTION('ref_axis',(-1.,0.,1.87133061054672E-16));
#17463=DIRECTION('',(-1.,0.,1.87133061054672E-16));
#17464=DIRECTION('',(0.,1.,0.));
#17465=DIRECTION('',(-1.,0.,1.87133061054672E-16));
#17466=DIRECTION('',(0.,1.,0.));
#17467=DIRECTION('center_axis',(1.,0.,0.));
#17468=DIRECTION('ref_axis',(0.,0.,-1.));
#17469=DIRECTION('',(0.,0.,-1.));
#17470=DIRECTION('',(0.,1.,0.));
#17471=DIRECTION('',(0.,0.,-1.));
#17472=DIRECTION('center_axis',(1.83697019872103E-16,0.,1.));
#17473=DIRECTION('ref_axis',(1.,0.,-1.83697019872103E-16));
#17474=DIRECTION('',(1.,0.,-1.83697019872103E-16));
#17475=DIRECTION('',(0.,1.,0.));
#17476=DIRECTION('',(1.,0.,-1.83697019872103E-16));
#17477=DIRECTION('center_axis',(-1.,0.,0.));
#17478=DIRECTION('ref_axis',(0.,0.,1.));
#17479=DIRECTION('',(0.,0.,1.));
#17480=DIRECTION('',(0.,0.,1.));
#17481=DIRECTION('center_axis',(0.,-1.,0.));
#17482=DIRECTION('ref_axis',(0.,0.,-1.));
#17483=DIRECTION('center_axis',(0.,-1.,0.));
#17484=DIRECTION('ref_axis',(0.,0.,-1.));
#17485=DIRECTION('center_axis',(-1.,0.,0.));
#17486=DIRECTION('ref_axis',(0.,0.,1.));
#17487=DIRECTION('',(0.,-1.18360663606093E-16,1.));
#17488=DIRECTION('',(0.,1.,9.62873847203288E-17));
#17489=DIRECTION('',(0.,-1.18360663606093E-16,1.));
#17490=DIRECTION('',(0.,1.,9.62873847203288E-17));
#17491=DIRECTION('center_axis',(-3.7224019040034E-16,9.62873847203288E-17,
-1.));
#17492=DIRECTION('ref_axis',(-1.,-2.72359540441036E-48,3.7224019040034E-16));
#17493=DIRECTION('',(-1.,0.,3.7224019040034E-16));
#17494=DIRECTION('',(0.,1.,9.62873847203288E-17));
#17495=DIRECTION('',(-1.,0.,3.7224019040034E-16));
#17496=DIRECTION('center_axis',(1.,0.,0.));
#17497=DIRECTION('ref_axis',(0.,0.,-1.));
#17498=DIRECTION('',(0.,1.18360663606093E-16,-1.));
#17499=DIRECTION('',(0.,1.,9.62873847203288E-17));
#17500=DIRECTION('',(0.,1.18360663606093E-16,-1.));
#17501=DIRECTION('center_axis',(0.,-9.62873847203288E-17,1.));
#17502=DIRECTION('ref_axis',(0.,-1.,-9.62873847203289E-17));
#17503=DIRECTION('',(1.,0.,0.));
#17504=DIRECTION('',(1.,0.,0.));
#17505=DIRECTION('center_axis',(0.,1.,1.18360663606093E-16));
#17506=DIRECTION('ref_axis',(0.,-1.18360663606093E-16,1.));
#17507=DIRECTION('center_axis',(0.,1.,1.18360663606093E-16));
#17508=DIRECTION('ref_axis',(0.,-1.18360663606093E-16,1.));
#17509=DIRECTION('center_axis',(1.,0.,0.));
#17510=DIRECTION('ref_axis',(0.,0.,1.));
#17511=DIRECTION('',(0.,-1.18360663606093E-16,1.));
#17512=DIRECTION('',(0.,1.,9.62873847203288E-17));
#17513=DIRECTION('',(0.,-1.18360663606093E-16,1.));
#17514=DIRECTION('',(0.,1.,9.62873847203288E-17));
#17515=DIRECTION('center_axis',(3.7224019040034E-16,9.62873847203288E-17,
-1.));
#17516=DIRECTION('ref_axis',(1.,-2.72359540441036E-48,3.7224019040034E-16));
#17517=DIRECTION('',(1.,0.,3.7224019040034E-16));
#17518=DIRECTION('',(1.,0.,3.7224019040034E-16));
#17519=DIRECTION('',(0.,1.,9.62873847203288E-17));
#17520=DIRECTION('center_axis',(-1.,0.,0.));
#17521=DIRECTION('ref_axis',(0.,0.,-1.));
#17522=DIRECTION('',(0.,1.18360663606093E-16,-1.));
#17523=DIRECTION('',(0.,1.18360663606093E-16,-1.));
#17524=DIRECTION('',(0.,1.,9.62873847203288E-17));
#17525=DIRECTION('center_axis',(0.,-9.62873847203288E-17,1.));
#17526=DIRECTION('ref_axis',(0.,-1.,-9.62873847203289E-17));
#17527=DIRECTION('',(-1.,0.,0.));
#17528=DIRECTION('',(-1.,0.,0.));
#17529=DIRECTION('center_axis',(0.,1.,1.18360663606093E-16));
#17530=DIRECTION('ref_axis',(0.,-1.18360663606093E-16,1.));
#17531=DIRECTION('center_axis',(0.,1.,1.18360663606093E-16));
#17532=DIRECTION('ref_axis',(0.,-1.18360663606093E-16,1.));
#17533=DIRECTION('axis',(0.,0.,1.));
#17534=DIRECTION('refdir',(1.,0.,0.));
#17535=DIRECTION('center_axis',(9.93056848476794E-32,1.,-3.33066907387547E-16));
#17536=DIRECTION('ref_axis',(7.13571935167128E-47,3.33066907387547E-16,
1.));
#17537=DIRECTION('center_axis',(9.93056848476794E-32,1.,-3.33066907387547E-16));
#17538=DIRECTION('ref_axis',(7.13571935167128E-47,3.33066907387547E-16,
1.));
#17539=DIRECTION('',(9.93056848476794E-32,1.,-3.33066907387547E-16));
#17540=DIRECTION('center_axis',(9.93056848476794E-32,1.,-3.33066907387547E-16));
#17541=DIRECTION('ref_axis',(6.61508746764379E-47,3.33066907387547E-16,
1.));
#17542=DIRECTION('center_axis',(9.93056848476794E-32,1.,-3.33066907387547E-16));
#17543=DIRECTION('ref_axis',(7.13571935167128E-47,3.33066907387547E-16,
1.));
#17544=DIRECTION('center_axis',(9.93056848476794E-32,1.,-3.33066907387547E-16));
#17545=DIRECTION('ref_axis',(7.13571935167128E-47,3.33066907387547E-16,
1.));
#17546=DIRECTION('',(9.93056848476794E-32,1.,-3.33066907387547E-16));
#17547=DIRECTION('center_axis',(9.93056848476794E-32,1.,-3.33066907387547E-16));
#17548=DIRECTION('ref_axis',(6.61508746764379E-47,3.33066907387547E-16,
1.));
#17549=DIRECTION('center_axis',(9.93056848476794E-32,1.,-3.33066907387547E-16));
#17550=DIRECTION('ref_axis',(7.13571935167129E-47,3.33066907387547E-16,
1.));
#17551=DIRECTION('center_axis',(9.93056848476794E-32,1.,-3.33066907387547E-16));
#17552=DIRECTION('ref_axis',(7.13571935167129E-47,3.33066907387547E-16,
1.));
#17553=DIRECTION('',(9.93056848476794E-32,1.,-3.33066907387547E-16));
#17554=DIRECTION('center_axis',(9.93056848476794E-32,1.,-3.33066907387547E-16));
#17555=DIRECTION('ref_axis',(6.61508746764379E-47,3.33066907387547E-16,
1.));
#17556=DIRECTION('center_axis',(9.93056848476794E-32,1.,-3.33066907387547E-16));
#17557=DIRECTION('ref_axis',(7.13571935167129E-47,3.33066907387547E-16,
1.));
#17558=DIRECTION('center_axis',(9.93056848476794E-32,1.,-3.33066907387547E-16));
#17559=DIRECTION('ref_axis',(7.13571935167129E-47,3.33066907387547E-16,
1.));
#17560=DIRECTION('',(9.93056848476794E-32,1.,-3.33066907387547E-16));
#17561=DIRECTION('center_axis',(9.93056848476794E-32,1.,-3.33066907387547E-16));
#17562=DIRECTION('ref_axis',(6.61508746764379E-47,3.33066907387547E-16,
1.));
#17563=DIRECTION('center_axis',(9.93056848476794E-32,1.,-3.33066907387547E-16));
#17564=DIRECTION('ref_axis',(7.13571935167128E-47,3.33066907387547E-16,
1.));
#17565=DIRECTION('center_axis',(9.93056848476794E-32,1.,-3.33066907387547E-16));
#17566=DIRECTION('ref_axis',(7.13571935167128E-47,3.33066907387547E-16,
1.));
#17567=DIRECTION('',(9.93056848476794E-32,1.,-3.33066907387547E-16));
#17568=DIRECTION('center_axis',(9.93056848476794E-32,1.,-3.33066907387547E-16));
#17569=DIRECTION('ref_axis',(6.61508746764379E-47,3.33066907387547E-16,
1.));
#17570=DIRECTION('center_axis',(9.93056848476794E-32,1.,-3.33066907387547E-16));
#17571=DIRECTION('ref_axis',(7.13571935167128E-47,3.33066907387547E-16,
1.));
#17572=DIRECTION('center_axis',(9.93056848476794E-32,1.,-3.33066907387547E-16));
#17573=DIRECTION('ref_axis',(7.13571935167128E-47,3.33066907387547E-16,
1.));
#17574=DIRECTION('',(9.93056848476794E-32,1.,-3.33066907387547E-16));
#17575=DIRECTION('center_axis',(9.93056848476794E-32,1.,-3.33066907387547E-16));
#17576=DIRECTION('ref_axis',(6.61508746764379E-47,3.33066907387547E-16,
1.));
#17577=DIRECTION('center_axis',(9.93056848476794E-32,1.,-3.33066907387547E-16));
#17578=DIRECTION('ref_axis',(7.13571935167128E-47,3.33066907387547E-16,
1.));
#17579=DIRECTION('center_axis',(9.93056848476794E-32,1.,-3.33066907387547E-16));
#17580=DIRECTION('ref_axis',(7.13571935167128E-47,3.33066907387547E-16,
1.));
#17581=DIRECTION('',(9.93056848476794E-32,1.,-3.33066907387547E-16));
#17582=DIRECTION('center_axis',(9.93056848476794E-32,1.,-3.33066907387547E-16));
#17583=DIRECTION('ref_axis',(6.61508746764379E-47,3.33066907387547E-16,
1.));
#17584=DIRECTION('center_axis',(9.93056848476794E-32,1.,-3.33066907387547E-16));
#17585=DIRECTION('ref_axis',(7.13571935167128E-47,3.33066907387547E-16,
1.));
#17586=DIRECTION('center_axis',(9.93056848476794E-32,1.,-3.33066907387547E-16));
#17587=DIRECTION('ref_axis',(7.13571935167128E-47,3.33066907387547E-16,
1.));
#17588=DIRECTION('',(9.93056848476794E-32,1.,-3.33066907387547E-16));
#17589=DIRECTION('center_axis',(9.93056848476794E-32,1.,-3.33066907387547E-16));
#17590=DIRECTION('ref_axis',(6.61508746764379E-47,3.33066907387547E-16,
1.));
#17591=DIRECTION('center_axis',(9.93056848476794E-32,1.,-3.33066907387547E-16));
#17592=DIRECTION('ref_axis',(7.13571935167128E-47,3.33066907387547E-16,
1.));
#17593=DIRECTION('center_axis',(9.93056848476794E-32,1.,-3.33066907387547E-16));
#17594=DIRECTION('ref_axis',(7.13571935167128E-47,3.33066907387547E-16,
1.));
#17595=DIRECTION('',(9.93056848476794E-32,1.,-3.33066907387547E-16));
#17596=DIRECTION('center_axis',(9.93056848476794E-32,1.,-3.33066907387547E-16));
#17597=DIRECTION('ref_axis',(6.61508746764379E-47,3.33066907387547E-16,
1.));
#17598=DIRECTION('center_axis',(9.93056848476794E-32,1.,-3.33066907387547E-16));
#17599=DIRECTION('ref_axis',(7.13571935167128E-47,3.33066907387547E-16,
1.));
#17600=DIRECTION('center_axis',(9.93056848476794E-32,1.,-3.33066907387547E-16));
#17601=DIRECTION('ref_axis',(7.13571935167128E-47,3.33066907387547E-16,
1.));
#17602=DIRECTION('',(9.93056848476794E-32,1.,-3.33066907387547E-16));
#17603=DIRECTION('center_axis',(9.93056848476794E-32,1.,-3.33066907387547E-16));
#17604=DIRECTION('ref_axis',(6.61508746764379E-47,3.33066907387547E-16,
1.));
#17605=DIRECTION('center_axis',(9.93056848476794E-32,1.,-3.33066907387547E-16));
#17606=DIRECTION('ref_axis',(7.13571935166959E-47,3.33066907387547E-16,
1.));
#17607=DIRECTION('center_axis',(9.93056848476794E-32,1.,-3.33066907387547E-16));
#17608=DIRECTION('ref_axis',(7.13571935166959E-47,3.33066907387547E-16,
1.));
#17609=DIRECTION('',(9.93056848476794E-32,1.,-3.33066907387547E-16));
#17610=DIRECTION('center_axis',(9.93056848476794E-32,1.,-3.33066907387547E-16));
#17611=DIRECTION('ref_axis',(6.61508746764379E-47,3.33066907387547E-16,
1.));
#17612=DIRECTION('center_axis',(9.93056848476794E-32,1.,-3.33066907387547E-16));
#17613=DIRECTION('ref_axis',(7.13571935167128E-47,3.33066907387547E-16,
1.));
#17614=DIRECTION('center_axis',(9.93056848476794E-32,1.,-3.33066907387547E-16));
#17615=DIRECTION('ref_axis',(7.13571935167128E-47,3.33066907387547E-16,
1.));
#17616=DIRECTION('',(9.93056848476794E-32,1.,-3.33066907387547E-16));
#17617=DIRECTION('center_axis',(9.93056848476794E-32,1.,-3.33066907387547E-16));
#17618=DIRECTION('ref_axis',(6.61508746764379E-47,3.33066907387547E-16,
1.));
#17619=DIRECTION('center_axis',(9.93056848476794E-32,1.,-3.33066907387547E-16));
#17620=DIRECTION('ref_axis',(7.13571935167128E-47,3.33066907387547E-16,
1.));
#17621=DIRECTION('center_axis',(9.93056848476794E-32,1.,-3.33066907387547E-16));
#17622=DIRECTION('ref_axis',(7.13571935167128E-47,3.33066907387547E-16,
1.));
#17623=DIRECTION('',(9.93056848476794E-32,1.,-3.33066907387547E-16));
#17624=DIRECTION('center_axis',(9.93056848476794E-32,1.,-3.33066907387547E-16));
#17625=DIRECTION('ref_axis',(6.61508746764379E-47,3.33066907387547E-16,
1.));
#17626=DIRECTION('center_axis',(9.93056848476794E-32,1.,-3.33066907387547E-16));
#17627=DIRECTION('ref_axis',(7.13571935167128E-47,3.33066907387547E-16,
1.));
#17628=DIRECTION('center_axis',(9.93056848476794E-32,1.,-3.33066907387547E-16));
#17629=DIRECTION('ref_axis',(7.13571935167128E-47,3.33066907387547E-16,
1.));
#17630=DIRECTION('',(9.93056848476794E-32,1.,-3.33066907387547E-16));
#17631=DIRECTION('center_axis',(9.93056848476794E-32,1.,-3.33066907387547E-16));
#17632=DIRECTION('ref_axis',(6.61508746764379E-47,3.33066907387547E-16,
1.));
#17633=DIRECTION('center_axis',(9.93056848476794E-32,1.,-3.33066907387547E-16));
#17634=DIRECTION('ref_axis',(7.13571935167128E-47,3.33066907387547E-16,
1.));
#17635=DIRECTION('center_axis',(9.93056848476794E-32,1.,-3.33066907387547E-16));
#17636=DIRECTION('ref_axis',(7.13571935167128E-47,3.33066907387547E-16,
1.));
#17637=DIRECTION('',(9.93056848476794E-32,1.,-3.33066907387547E-16));
#17638=DIRECTION('center_axis',(9.93056848476794E-32,1.,-3.33066907387547E-16));
#17639=DIRECTION('ref_axis',(6.61508746764379E-47,3.33066907387547E-16,
1.));
#17640=DIRECTION('center_axis',(9.93056848476794E-32,1.,-3.33066907387547E-16));
#17641=DIRECTION('ref_axis',(6.64176120743267E-47,3.33066907387547E-16,
1.));
#17642=DIRECTION('center_axis',(9.93056848476794E-32,1.,-3.33066907387547E-16));
#17643=DIRECTION('ref_axis',(6.64176120743267E-47,3.33066907387547E-16,
1.));
#17644=DIRECTION('',(9.93056848476794E-32,1.,-3.33066907387547E-16));
#17645=DIRECTION('center_axis',(9.93056848476794E-32,1.,-3.33066907387547E-16));
#17646=DIRECTION('ref_axis',(6.61508746764379E-47,3.33066907387547E-16,
1.));
#17647=DIRECTION('center_axis',(9.93056848476794E-32,1.,-3.33066907387547E-16));
#17648=DIRECTION('ref_axis',(6.55317088808553E-47,3.33066907387547E-16,
1.));
#17649=DIRECTION('center_axis',(9.93056848476794E-32,1.,-3.33066907387547E-16));
#17650=DIRECTION('ref_axis',(6.55317088808553E-47,3.33066907387547E-16,
1.));
#17651=DIRECTION('',(9.93056848476794E-32,1.,-3.33066907387547E-16));
#17652=DIRECTION('center_axis',(9.93056848476794E-32,1.,-3.33066907387547E-16));
#17653=DIRECTION('ref_axis',(6.61508746764379E-47,3.33066907387547E-16,
1.));
#17654=DIRECTION('center_axis',(9.93056848476794E-32,1.,-3.33066907387547E-16));
#17655=DIRECTION('ref_axis',(7.13571935167128E-47,3.33066907387547E-16,
1.));
#17656=DIRECTION('center_axis',(9.93056848476794E-32,1.,-3.33066907387547E-16));
#17657=DIRECTION('ref_axis',(7.13571935167128E-47,3.33066907387547E-16,
1.));
#17658=DIRECTION('',(9.93056848476794E-32,1.,-3.33066907387547E-16));
#17659=DIRECTION('center_axis',(9.93056848476794E-32,1.,-3.33066907387547E-16));
#17660=DIRECTION('ref_axis',(6.61508746764379E-47,3.33066907387547E-16,
1.));
#17661=DIRECTION('center_axis',(1.,9.93056848476794E-32,1.97215226305253E-31));
#17662=DIRECTION('ref_axis',(1.97215226305253E-31,3.33066907387547E-16,
-1.));
#17663=DIRECTION('',(1.97215226305253E-31,3.33066907387547E-16,-1.));
#17664=DIRECTION('',(9.93056848476794E-32,1.,-3.33066907387547E-16));
#17665=DIRECTION('',(1.97215226305253E-31,3.33066907387547E-16,-1.));
#17666=DIRECTION('',(9.93056848476794E-32,1.,-3.33066907387547E-16));
#17667=DIRECTION('center_axis',(2.2186712959341E-31,-3.33066907387547E-16,
1.));
#17668=DIRECTION('ref_axis',(1.,9.93056848476795E-32,-2.2186712959341E-31));
#17669=DIRECTION('',(1.,9.93056848476795E-32,-2.2186712959341E-31));
#17670=DIRECTION('',(9.93056848476794E-32,1.,-3.33066907387547E-16));
#17671=DIRECTION('',(1.,9.93056848476795E-32,-2.2186712959341E-31));
#17672=DIRECTION('center_axis',(-1.,-9.93056848476794E-32,-1.97215226305253E-31));
#17673=DIRECTION('ref_axis',(-1.97215226305253E-31,-3.33066907387547E-16,
1.));
#17674=DIRECTION('',(-1.97215226305253E-31,-3.33066907387547E-16,1.));
#17675=DIRECTION('',(9.93056848476794E-32,1.,-3.33066907387547E-16));
#17676=DIRECTION('',(-1.97215226305253E-31,-3.33066907387547E-16,1.));
#17677=DIRECTION('center_axis',(-2.2186712959341E-31,3.33066907387547E-16,
-1.));
#17678=DIRECTION('ref_axis',(-1.,-9.93056848476795E-32,2.2186712959341E-31));
#17679=DIRECTION('',(-1.,-9.93056848476795E-32,2.2186712959341E-31));
#17680=DIRECTION('',(-1.,-9.93056848476795E-32,2.2186712959341E-31));
#17681=DIRECTION('center_axis',(-9.93056848476793E-32,-1.,-3.33066907387547E-16));
#17682=DIRECTION('ref_axis',(1.97215226305253E-31,3.33066907387547E-16,
-1.));
#17683=DIRECTION('center_axis',(-9.93056848476793E-32,-1.,-3.33066907387547E-16));
#17684=DIRECTION('ref_axis',(1.97215226305253E-31,3.33066907387547E-16,
-1.));
#17685=DIRECTION('center_axis',(-6.62037898984529E-32,-1.,2.22044604925031E-16));
#17686=DIRECTION('ref_axis',(-2.81594457665554E-47,-2.22044604925031E-16,
-1.));
#17687=DIRECTION('center_axis',(6.62037898984529E-32,1.,-1.60812264967664E-16));
#17688=DIRECTION('ref_axis',(2.94003887450835E-47,1.60812264967664E-16,
1.));
#17689=DIRECTION('',(6.62037898984529E-32,1.,-2.22044604925031E-16));
#17690=DIRECTION('center_axis',(6.62037898984529E-32,1.,-1.60812264967664E-16));
#17691=DIRECTION('ref_axis',(2.41056327970272E-47,1.60812264967664E-16,
1.));
#17692=DIRECTION('center_axis',(-6.62037898984529E-32,-1.,2.22044604925031E-16));
#17693=DIRECTION('ref_axis',(-2.98319463103498E-47,-2.22044604925031E-16,
-1.));
#17694=DIRECTION('center_axis',(6.62037898984529E-32,1.,-1.60812264967664E-16));
#17695=DIRECTION('ref_axis',(2.57781333408216E-47,1.60812264967664E-16,
1.));
#17696=DIRECTION('',(-6.62037898984529E-32,-1.,2.22044604925031E-16));
#17697=DIRECTION('center_axis',(6.62037898984529E-32,1.,-1.60812264967664E-16));
#17698=DIRECTION('ref_axis',(2.94003887450835E-47,1.60812264967664E-16,
1.));
#17699=DIRECTION('center_axis',(6.62037898984529E-32,1.,2.83276944882399E-16));
#17700=DIRECTION('ref_axis',(-1.4791141972894E-31,-2.83276944882399E-16,
1.));
#17701=DIRECTION('center_axis',(6.62037898984529E-32,1.,2.83276944882399E-16));
#17702=DIRECTION('ref_axis',(-1.4791141972894E-31,-2.83276944882399E-16,
1.));
#17703=DIRECTION('center_axis',(5.74253288599218E-16,-1.,2.22044604925031E-16));
#17704=DIRECTION('ref_axis',(1.,5.74253288599218E-16,7.6798984248757E-32));
#17705=DIRECTION('center_axis',(-5.74253288599218E-16,1.,-1.60812264967664E-16));
#17706=DIRECTION('ref_axis',(-1.,-5.74253288599218E-16,1.83632660503434E-32));
#17707=DIRECTION('',(-5.74253288599218E-16,1.,-2.22044604925031E-16));
#17708=DIRECTION('center_axis',(-5.74253288599218E-16,1.,-1.60812264967664E-16));
#17709=DIRECTION('ref_axis',(-1.,-5.74253288599218E-16,-5.56204399040829E-32));
#17710=DIRECTION('center_axis',(5.74253288599218E-16,-1.,2.22044604925031E-16));
#17711=DIRECTION('ref_axis',(1.,5.74253288599218E-16,1.07225475232373E-31));
#17712=DIRECTION('center_axis',(-5.74253288599218E-16,1.,-1.60812264967664E-16));
#17713=DIRECTION('ref_axis',(-1.,-5.74253288599218E-16,-7.76563408967936E-32));
#17714=DIRECTION('',(5.74253288599218E-16,-1.,2.22044604925031E-16));
#17715=DIRECTION('center_axis',(-5.74253288599218E-16,1.,-1.60812264967664E-16));
#17716=DIRECTION('ref_axis',(-1.,-5.74253288599219E-16,7.34531555398823E-33));
#17717=DIRECTION('center_axis',(-5.74253288599219E-16,1.,-1.60812264967664E-16));
#17718=DIRECTION('ref_axis',(-1.,-5.74253288599219E-16,2.95822839457879E-31));
#17719=DIRECTION('center_axis',(-5.74253288599219E-16,1.,-1.60812264967664E-16));
#17720=DIRECTION('ref_axis',(-1.,-5.74253288599219E-16,2.95822839457879E-31));
#17721=DIRECTION('center_axis',(6.62037898984529E-32,1.,-1.60812264967664E-16));
#17722=DIRECTION('ref_axis',(1.06463814030135E-47,1.60812264967664E-16,
1.));
#17723=DIRECTION('center_axis',(6.62037898984529E-32,1.,-1.60812264967664E-16));
#17724=DIRECTION('ref_axis',(1.06463814030135E-47,1.60812264967664E-16,
1.));
#17725=DIRECTION('',(6.62037898984529E-32,1.,-1.60812264967664E-16));
#17726=DIRECTION('center_axis',(6.62037898984529E-32,1.,-1.60812264967664E-16));
#17727=DIRECTION('ref_axis',(1.06463814030135E-47,1.60812264967664E-16,
1.));
#17728=DIRECTION('center_axis',(6.62037898984529E-32,1.,-1.60812264967664E-16));
#17729=DIRECTION('ref_axis',(1.06463814030135E-47,1.60812264967664E-16,
1.));
#17730=DIRECTION('center_axis',(6.62037898984529E-32,1.,-1.60812264967664E-16));
#17731=DIRECTION('ref_axis',(1.06463814030135E-47,1.60812264967664E-16,
1.));
#17732=DIRECTION('',(6.62037898984529E-32,1.,-1.60812264967664E-16));
#17733=DIRECTION('center_axis',(6.62037898984529E-32,1.,-1.60812264967664E-16));
#17734=DIRECTION('ref_axis',(1.06463814030135E-47,1.60812264967664E-16,
1.));
#17735=DIRECTION('center_axis',(6.62037898984529E-32,1.,-1.60812264967664E-16));
#17736=DIRECTION('ref_axis',(1.06463814030135E-47,1.60812264967664E-16,
1.));
#17737=DIRECTION('center_axis',(6.62037898984529E-32,1.,-1.60812264967664E-16));
#17738=DIRECTION('ref_axis',(1.06463814030135E-47,1.60812264967664E-16,
1.));
#17739=DIRECTION('',(6.62037898984529E-32,1.,-1.60812264967664E-16));
#17740=DIRECTION('center_axis',(6.62037898984529E-32,1.,-1.60812264967664E-16));
#17741=DIRECTION('ref_axis',(1.06463814030135E-47,1.60812264967664E-16,
1.));
#17742=DIRECTION('center_axis',(6.62037898984529E-32,1.,-1.60812264967664E-16));
#17743=DIRECTION('ref_axis',(1.06463814030135E-47,1.60812264967664E-16,
1.));
#17744=DIRECTION('center_axis',(6.62037898984529E-32,1.,-1.60812264967664E-16));
#17745=DIRECTION('ref_axis',(1.06463814030135E-47,1.60812264967664E-16,
1.));
#17746=DIRECTION('',(6.62037898984529E-32,1.,-1.60812264967664E-16));
#17747=DIRECTION('center_axis',(6.62037898984529E-32,1.,-1.60812264967664E-16));
#17748=DIRECTION('ref_axis',(1.06463814030135E-47,1.60812264967664E-16,
1.));
#17749=DIRECTION('center_axis',(6.62037898984529E-32,1.,-1.60812264967664E-16));
#17750=DIRECTION('ref_axis',(1.06463814030135E-47,1.60812264967664E-16,
1.));
#17751=DIRECTION('center_axis',(6.62037898984529E-32,1.,-1.60812264967664E-16));
#17752=DIRECTION('ref_axis',(1.06463814030135E-47,1.60812264967664E-16,
1.));
#17753=DIRECTION('',(6.62037898984529E-32,1.,-1.60812264967664E-16));
#17754=DIRECTION('center_axis',(6.62037898984529E-32,1.,-1.60812264967664E-16));
#17755=DIRECTION('ref_axis',(1.06463814030135E-47,1.60812264967664E-16,
1.));
#17756=DIRECTION('center_axis',(6.62037898984529E-32,1.,-1.60812264967664E-16));
#17757=DIRECTION('ref_axis',(1.06463814030135E-47,1.60812264967664E-16,
1.));
#17758=DIRECTION('center_axis',(6.62037898984529E-32,1.,-1.60812264967664E-16));
#17759=DIRECTION('ref_axis',(1.06463814030135E-47,1.60812264967664E-16,
1.));
#17760=DIRECTION('',(6.62037898984529E-32,1.,-1.60812264967664E-16));
#17761=DIRECTION('center_axis',(6.62037898984529E-32,1.,-1.60812264967664E-16));
#17762=DIRECTION('ref_axis',(1.06463814030135E-47,1.60812264967664E-16,
1.));
#17763=DIRECTION('center_axis',(6.62037898984529E-32,1.,-1.60812264967664E-16));
#17764=DIRECTION('ref_axis',(1.06463814030135E-47,1.60812264967664E-16,
1.));
#17765=DIRECTION('center_axis',(6.62037898984529E-32,1.,-1.60812264967664E-16));
#17766=DIRECTION('ref_axis',(1.06463814030135E-47,1.60812264967664E-16,
1.));
#17767=DIRECTION('',(6.62037898984529E-32,1.,-1.60812264967664E-16));
#17768=DIRECTION('center_axis',(6.62037898984529E-32,1.,-1.60812264967664E-16));
#17769=DIRECTION('ref_axis',(1.06463814030135E-47,1.60812264967664E-16,
1.));
#17770=DIRECTION('center_axis',(6.62037898984529E-32,1.,-1.60812264967664E-16));
#17771=DIRECTION('ref_axis',(1.06463814030135E-47,1.60812264967664E-16,
1.));
#17772=DIRECTION('center_axis',(6.62037898984529E-32,1.,-1.60812264967664E-16));
#17773=DIRECTION('ref_axis',(1.06463814030135E-47,1.60812264967664E-16,
1.));
#17774=DIRECTION('',(6.62037898984529E-32,1.,-1.60812264967664E-16));
#17775=DIRECTION('center_axis',(6.62037898984529E-32,1.,-1.60812264967664E-16));
#17776=DIRECTION('ref_axis',(1.06463814030135E-47,1.60812264967664E-16,
1.));
#17777=DIRECTION('center_axis',(6.62037898984529E-32,1.,-1.60812264967664E-16));
#17778=DIRECTION('ref_axis',(1.06463814030135E-47,1.60812264967664E-16,
1.));
#17779=DIRECTION('center_axis',(6.62037898984529E-32,1.,-1.60812264967664E-16));
#17780=DIRECTION('ref_axis',(1.06463814030135E-47,1.60812264967664E-16,
1.));
#17781=DIRECTION('',(6.62037898984529E-32,1.,-1.60812264967664E-16));
#17782=DIRECTION('center_axis',(6.62037898984529E-32,1.,-1.60812264967664E-16));
#17783=DIRECTION('ref_axis',(1.06463814030135E-47,1.60812264967664E-16,
1.));
#17784=DIRECTION('center_axis',(6.62037898984529E-32,1.,-1.60812264967664E-16));
#17785=DIRECTION('ref_axis',(1.06463814030135E-47,1.60812264967664E-16,
1.));
#17786=DIRECTION('center_axis',(6.62037898984529E-32,1.,-1.60812264967664E-16));
#17787=DIRECTION('ref_axis',(1.06463814030135E-47,1.60812264967664E-16,
1.));
#17788=DIRECTION('',(6.62037898984529E-32,1.,-1.60812264967664E-16));
#17789=DIRECTION('center_axis',(6.62037898984529E-32,1.,-1.60812264967664E-16));
#17790=DIRECTION('ref_axis',(1.06463814030135E-47,1.60812264967664E-16,
1.));
#17791=DIRECTION('center_axis',(6.62037898984529E-32,1.,-1.60812264967664E-16));
#17792=DIRECTION('ref_axis',(1.06463814030135E-47,1.60812264967664E-16,
1.));
#17793=DIRECTION('center_axis',(6.62037898984529E-32,1.,-1.60812264967664E-16));
#17794=DIRECTION('ref_axis',(1.06463814030135E-47,1.60812264967664E-16,
1.));
#17795=DIRECTION('',(6.62037898984529E-32,1.,-1.60812264967664E-16));
#17796=DIRECTION('center_axis',(6.62037898984529E-32,1.,-1.60812264967664E-16));
#17797=DIRECTION('ref_axis',(1.06463814030135E-47,1.60812264967664E-16,
1.));
#17798=DIRECTION('center_axis',(6.62037898984529E-32,1.,-1.60812264967664E-16));
#17799=DIRECTION('ref_axis',(1.06463814030135E-47,1.60812264967664E-16,
1.));
#17800=DIRECTION('center_axis',(6.62037898984529E-32,1.,-1.60812264967664E-16));
#17801=DIRECTION('ref_axis',(1.06463814030135E-47,1.60812264967664E-16,
1.));
#17802=DIRECTION('',(6.62037898984529E-32,1.,-1.60812264967664E-16));
#17803=DIRECTION('center_axis',(6.62037898984529E-32,1.,-1.60812264967664E-16));
#17804=DIRECTION('ref_axis',(1.06463814030135E-47,1.60812264967664E-16,
1.));
#17805=DIRECTION('center_axis',(6.62037898984529E-32,1.,-1.60812264967664E-16));
#17806=DIRECTION('ref_axis',(3.06194715830974E-47,1.60812264967664E-16,
1.));
#17807=DIRECTION('center_axis',(6.62037898984529E-32,1.,-1.60812264967664E-16));
#17808=DIRECTION('ref_axis',(3.06194715830974E-47,1.60812264967664E-16,
1.));
#17809=DIRECTION('',(6.62037898984529E-32,1.,-1.60812264967664E-16));
#17810=DIRECTION('center_axis',(6.62037898984529E-32,1.,-1.60812264967664E-16));
#17811=DIRECTION('ref_axis',(2.39617748564028E-47,1.60812264967664E-16,
1.));
#17812=DIRECTION('center_axis',(6.62037898984529E-32,1.,-1.60812264967664E-16));
#17813=DIRECTION('ref_axis',(2.8750069053927E-47,1.60812264967664E-16,1.));
#17814=DIRECTION('center_axis',(6.62037898984529E-32,1.,-1.60812264967664E-16));
#17815=DIRECTION('ref_axis',(2.8750069053927E-47,1.60812264967664E-16,1.));
#17816=DIRECTION('',(-6.62037898984529E-32,-1.,1.60812264967664E-16));
#17817=DIRECTION('center_axis',(6.62037898984529E-32,1.,-1.60812264967664E-16));
#17818=DIRECTION('ref_axis',(2.8750069053927E-47,1.60812264967664E-16,1.));
#17819=DIRECTION('center_axis',(6.62037898984529E-32,1.,2.83276944882399E-16));
#17820=DIRECTION('ref_axis',(-1.4791141972894E-31,-2.83276944882399E-16,
1.));
#17821=DIRECTION('center_axis',(6.62037898984529E-32,1.,2.83276944882399E-16));
#17822=DIRECTION('ref_axis',(-1.4791141972894E-31,-2.83276944882399E-16,
1.));
#17823=DIRECTION('center_axis',(-5.74253288599218E-16,1.,-1.60812264967664E-16));
#17824=DIRECTION('ref_axis',(-1.,-5.74253288599219E-16,9.23469720047697E-32));
#17825=DIRECTION('center_axis',(-5.74253288599218E-16,1.,-1.60812264967664E-16));
#17826=DIRECTION('ref_axis',(-1.,-5.74253288599219E-16,9.23469720047697E-32));
#17827=DIRECTION('',(-5.74253288599219E-16,1.,-1.60812264967664E-16));
#17828=DIRECTION('center_axis',(-5.74253288599218E-16,1.,-1.60812264967664E-16));
#17829=DIRECTION('ref_axis',(-1.,-5.74253288599219E-16,9.23469720047697E-32));
#17830=DIRECTION('center_axis',(-5.74253288599218E-16,1.,-1.60812264967664E-16));
#17831=DIRECTION('ref_axis',(-1.,-5.74253288599219E-16,9.23469720047697E-32));
#17832=DIRECTION('center_axis',(-5.74253288599218E-16,1.,-1.60812264967664E-16));
#17833=DIRECTION('ref_axis',(-1.,-5.74253288599219E-16,9.23469720047697E-32));
#17834=DIRECTION('',(-5.74253288599219E-16,1.,-1.60812264967664E-16));
#17835=DIRECTION('center_axis',(-5.74253288599218E-16,1.,-1.60812264967664E-16));
#17836=DIRECTION('ref_axis',(-1.,-5.74253288599219E-16,9.23469720047697E-32));
#17837=DIRECTION('center_axis',(-5.74253288599218E-16,1.,-1.60812264967664E-16));
#17838=DIRECTION('ref_axis',(-1.,-5.74253288599219E-16,9.23469720047697E-32));
#17839=DIRECTION('center_axis',(-5.74253288599218E-16,1.,-1.60812264967664E-16));
#17840=DIRECTION('ref_axis',(-1.,-5.74253288599219E-16,9.23469720047697E-32));
#17841=DIRECTION('',(-5.74253288599219E-16,1.,-1.60812264967664E-16));
#17842=DIRECTION('center_axis',(-5.74253288599218E-16,1.,-1.60812264967664E-16));
#17843=DIRECTION('ref_axis',(-1.,-5.74253288599219E-16,9.23469720047697E-32));
#17844=DIRECTION('center_axis',(-5.74253288599218E-16,1.,-1.60812264967664E-16));
#17845=DIRECTION('ref_axis',(-1.,-5.74253288599219E-16,9.23469720047697E-32));
#17846=DIRECTION('center_axis',(-5.74253288599218E-16,1.,-1.60812264967664E-16));
#17847=DIRECTION('ref_axis',(-1.,-5.74253288599219E-16,9.23469720047697E-32));
#17848=DIRECTION('',(-5.74253288599219E-16,1.,-1.60812264967664E-16));
#17849=DIRECTION('center_axis',(-5.74253288599218E-16,1.,-1.60812264967664E-16));
#17850=DIRECTION('ref_axis',(-1.,-5.74253288599219E-16,9.23469720047697E-32));
#17851=DIRECTION('center_axis',(-5.74253288599218E-16,1.,-1.60812264967664E-16));
#17852=DIRECTION('ref_axis',(-1.,-5.74253288599219E-16,-5.16348660671831E-32));
#17853=DIRECTION('center_axis',(-5.74253288599218E-16,1.,-1.60812264967664E-16));
#17854=DIRECTION('ref_axis',(-1.,-5.74253288599219E-16,-5.16348660671831E-32));
#17855=DIRECTION('',(-5.74253288599219E-16,1.,-1.60812264967664E-16));
#17856=DIRECTION('center_axis',(-5.74253288599218E-16,1.,-1.60812264967664E-16));
#17857=DIRECTION('ref_axis',(-1.,-5.74253288599219E-16,-5.16348660671831E-32));
#17858=DIRECTION('center_axis',(-5.74253288599218E-16,1.,-1.60812264967664E-16));
#17859=DIRECTION('ref_axis',(-1.,-5.74253288599219E-16,-2.51118958960339E-32));
#17860=DIRECTION('center_axis',(-5.74253288599218E-16,1.,-1.60812264967664E-16));
#17861=DIRECTION('ref_axis',(-1.,-5.74253288599219E-16,-2.51118958960339E-32));
#17862=DIRECTION('',(5.74253288599219E-16,-1.,1.60812264967664E-16));
#17863=DIRECTION('center_axis',(-5.74253288599218E-16,1.,-1.60812264967664E-16));
#17864=DIRECTION('ref_axis',(-1.,-5.74253288599219E-16,-2.51118958960339E-32));
#17865=DIRECTION('center_axis',(-5.74253288599219E-16,1.,-1.60812264967664E-16));
#17866=DIRECTION('ref_axis',(-1.,-5.74253288599219E-16,2.95822839457879E-31));
#17867=DIRECTION('center_axis',(-5.74253288599219E-16,1.,-1.60812264967664E-16));
#17868=DIRECTION('ref_axis',(-1.,-5.74253288599219E-16,2.95822839457879E-31));
#17869=DIRECTION('axis',(0.,0.,1.));
#17870=DIRECTION('refdir',(1.,0.,0.));
#17871=DIRECTION('axis',(0.,0.,1.));
#17872=DIRECTION('refdir',(1.,0.,0.));
#17873=DIRECTION('center_axis',(0.707106781186548,-9.87540052432906E-15,
-0.707106781186548));
#17874=DIRECTION('ref_axis',(-0.707106781186548,-7.45999389735652E-32,-0.707106781186548));
#17875=DIRECTION('',(-6.98296267768627E-15,-1.,6.98296267768627E-15));
#17876=DIRECTION('',(-0.707106781186547,-5.66993775627602E-31,-0.707106781186547));
#17877=DIRECTION('',(-4.37653262704222E-17,1.,-1.4009690681643E-14));
#17878=DIRECTION('',(0.707106781186547,-4.93770026216453E-15,0.707106781186547));
#17879=DIRECTION('center_axis',(-0.707106781186503,5.10171234491475E-14,
0.707106781186592));
#17880=DIRECTION('ref_axis',(0.707106781186592,4.06006286315216E-13,0.707106781186503));
#17881=DIRECTION('',(2.82341939598128E-17,-1.,1.39941595493323E-14));
#17882=DIRECTION('center_axis',(0.707106781186548,-8.6849455722553E-15,
-0.707106781186547));
#17883=DIRECTION('ref_axis',(0.707106781186547,1.24067126081198E-13,0.707106781186548));
#17884=DIRECTION('',(0.707106781186547,-1.10208153157725E-17,0.707106781186547));
#17885=DIRECTION('center_axis',(-0.707106781186547,1.44247999773054E-14,
0.707106781186548));
#17886=DIRECTION('ref_axis',(0.707106781186548,2.09065760029798E-13,0.707106781186547));
#17887=DIRECTION('center_axis',(0.707106781186548,9.87540052432906E-15,
0.707106781186547));
#17888=DIRECTION('ref_axis',(0.707106781186547,-7.45999389735652E-32,-0.707106781186548));
#17889=DIRECTION('',(0.707106781186548,5.66993775627602E-31,-0.707106781186548));
#17890=DIRECTION('',(6.98296267768627E-15,1.,-2.09488880330588E-14));
#17891=DIRECTION('center_axis',(-0.70710678118655,-2.33342352574054E-15,
-0.707106781186545));
#17892=DIRECTION('ref_axis',(0.707106781186545,-3.39200069252924E-13,-0.70710678118655));
#17893=DIRECTION('',(-0.707106781186548,1.10208153157725E-17,0.707106781186548));
#17894=DIRECTION('center_axis',(0.707106781186561,3.37058601970852E-14,
0.707106781186534));
#17895=DIRECTION('ref_axis',(0.707106781186534,2.01365616121726E-13,-0.707106781186561));
#17896=DIRECTION('',(-2.82341939598121E-17,1.,-1.39376911614127E-14));
#17897=DIRECTION('center_axis',(-0.707106781186548,-1.42126705658744E-14,
-0.707106781186547));
#17898=DIRECTION('ref_axis',(0.707106781186547,-3.72911172953344E-14,-0.707106781186548));
#17899=DIRECTION('',(-0.707106781186548,4.93770026216453E-15,0.707106781186548));
#17900=DIRECTION('',(4.37653262704214E-17,-1.,1.39221600291021E-14));
#17901=DIRECTION('center_axis',(-7.88860896404804E-31,1.,2.05680528781315E-77));
#17902=DIRECTION('ref_axis',(-1.,-7.88860896404804E-31,-1.16649095722751E-39));
#17903=DIRECTION('',(1.16649072924818E-39,0.,1.));
#17904=DIRECTION('',(1.16649072924818E-39,0.,1.));
#17905=DIRECTION('center_axis',(1.,4.37653262704214E-17,-3.42470776094434E-41));
#17906=DIRECTION('ref_axis',(-4.37653262704214E-17,1.,-4.04863581862828E-74));
#17907=DIRECTION('',(1.16649072924818E-39,0.,1.));
#17908=DIRECTION('center_axis',(-6.98296267768627E-15,-1.,0.));
#17909=DIRECTION('ref_axis',(1.,-6.98296267768627E-15,1.76663133728356E-39));
#17910=DIRECTION('',(1.16649072924818E-39,0.,1.));
#17911=DIRECTION('center_axis',(1.16649072924818E-39,0.,1.));
#17912=DIRECTION('ref_axis',(1.,0.,-1.16649072924818E-39));
#17913=DIRECTION('',(1.16649072924818E-39,0.,1.));
#17914=DIRECTION('center_axis',(-1.,-2.82341939598121E-17,-1.14077343289525E-39));
#17915=DIRECTION('ref_axis',(2.82341939598121E-17,-1.,9.93228473184302E-73));
#17916=DIRECTION('',(1.16649072924818E-39,0.,1.));
#17917=DIRECTION('center_axis',(1.16649072924818E-39,0.,1.));
#17918=DIRECTION('ref_axis',(1.,0.,-1.16649072924818E-39));
#17919=DIRECTION('',(1.16649072924818E-39,0.,1.));
#17920=DIRECTION('center_axis',(-1.55857864879746E-17,-1.,0.));
#17921=DIRECTION('ref_axis',(1.,-1.55857864879746E-17,1.48465414644535E-38));
#17922=DIRECTION('',(1.16649072924818E-39,0.,1.));
#17923=DIRECTION('center_axis',(1.16649072924818E-39,0.,1.));
#17924=DIRECTION('ref_axis',(1.,0.,-1.16649072924818E-39));
#17925=DIRECTION('',(1.16649072924818E-39,0.,1.));
#17926=DIRECTION('center_axis',(-1.,6.98296267768627E-15,1.17210418944755E-39));
#17927=DIRECTION('ref_axis',(-6.98296267768627E-15,-1.,1.56236334624413E-70));
#17928=DIRECTION('center_axis',(-0.707106781186547,9.76996261670137E-15,
0.707106781186548));
#17929=DIRECTION('ref_axis',(0.707106781186548,-1.25110045007797E-31,0.707106781186547));
#17930=DIRECTION('',(2.09488879640879E-14,1.,6.93889390390723E-15));
#17931=DIRECTION('center_axis',(0.707106781186556,6.78814116579064E-15,
-0.707106781186539));
#17932=DIRECTION('ref_axis',(0.707106781186539,8.68490834600899E-15,0.707106781186556));
#17933=DIRECTION('',(-0.707106781186548,5.55111512312578E-17,-0.707106781186548));
#17934=DIRECTION('center_axis',(-0.707106781186566,-1.56122235882211E-14,
0.707106781186529));
#17935=DIRECTION('ref_axis',(0.707106781186529,7.38317989499037E-14,0.707106781186566));
#17936=DIRECTION('',(1.39376911160448E-14,1.,0.));
#17937=DIRECTION('center_axis',(0.707106781186543,-2.20614587888198E-14,
-0.707106781186552));
#17938=DIRECTION('ref_axis',(0.707106781186552,5.51055984241866E-14,0.707106781186543));
#17939=DIRECTION('',(-0.707106781186548,4.94049245958195E-15,-0.707106781186548));
#17940=DIRECTION('',(-1.39221599728635E-14,-1.,0.));
#17941=DIRECTION('',(0.707106781186548,0.,0.707106781186548));
#17942=DIRECTION('center_axis',(0.707106781186548,-4.94049245958195E-15,
0.707106781186548));
#17943=DIRECTION('ref_axis',(0.707106781186548,5.55111512312576E-17,-0.707106781186548));
#17944=DIRECTION('',(0.707106781186547,5.55111512312578E-17,-0.707106781186547));
#17945=DIRECTION('',(7.02672793828483E-15,1.,0.));
#17946=DIRECTION('',(-0.707106781186547,-4.99600361081321E-15,0.707106781186547));
#17947=DIRECTION('center_axis',(-0.707106781186547,8.69730586866938E-15,
-0.707106781186548));
#17948=DIRECTION('ref_axis',(0.707106781186548,1.59821939493797E-13,-0.707106781186547));
#17949=DIRECTION('',(-7.01119682157331E-15,-1.,0.));
#17950=DIRECTION('center_axis',(0.707106781186539,2.04716574203159E-14,
0.707106781186556));
#17951=DIRECTION('ref_axis',(0.707106781186556,4.33830102985163E-13,-0.707106781186539));
#17952=DIRECTION('',(-0.707106781186547,-5.55111512312578E-17,0.707106781186547));
#17953=DIRECTION('center_axis',(-0.707106781186547,8.69730586866915E-15,
-0.707106781186548));
#17954=DIRECTION('ref_axis',(0.707106781186548,-6.72197636050009E-14,-0.707106781186547));
#17955=DIRECTION('',(7.94093388050907E-23,-1.,-6.93889390390723E-15));
#17956=DIRECTION('center_axis',(-5.29395592033938E-23,1.,-1.40129846432482E-45));
#17957=DIRECTION('ref_axis',(-2.64697796016969E-23,0.,1.));
#17958=DIRECTION('',(-1.,5.29395592033937E-23,2.64697796016969E-23));
#17959=DIRECTION('',(-1.,5.29395592033937E-23,2.64697796016969E-23));
#17960=DIRECTION('center_axis',(-2.64697796016969E-23,-1.40129846432482E-45,
1.));
#17961=DIRECTION('ref_axis',(5.29395592033938E-23,-1.,0.));
#17962=DIRECTION('',(-1.,5.29395592033937E-23,2.64697796016969E-23));
#17963=DIRECTION('center_axis',(7.94093388050907E-23,-1.,-7.04991620636974E-15));
#17964=DIRECTION('ref_axis',(2.64697796016969E-23,7.04991620636974E-15,
-1.));
#17965=DIRECTION('',(-1.,5.29395592033937E-23,2.64697796016969E-23));
#17966=DIRECTION('center_axis',(-1.,5.29395592033937E-23,2.64697796016969E-23));
#17967=DIRECTION('ref_axis',(2.64697796016969E-23,-1.40129846432482E-45,
1.));
#17968=DIRECTION('',(-1.,5.29395592033937E-23,2.64697796016969E-23));
#17969=DIRECTION('center_axis',(2.64697796016969E-23,1.40129846432482E-45,
-1.));
#17970=DIRECTION('ref_axis',(-5.29395592033938E-23,1.,0.));
#17971=DIRECTION('',(-1.,5.29395592033937E-23,2.64697796016969E-23));
#17972=DIRECTION('center_axis',(-1.,5.29395592033937E-23,2.64697796016969E-23));
#17973=DIRECTION('ref_axis',(2.64697796016969E-23,-1.40129846432481E-45,
1.));
#17974=DIRECTION('',(-1.,5.29395592033937E-23,2.64697796016969E-23));
#17975=DIRECTION('center_axis',(5.29395592033938E-23,-1.,1.40129846432482E-45));
#17976=DIRECTION('ref_axis',(2.64697796016969E-23,0.,-1.));
#17977=DIRECTION('',(-1.,5.29395592033937E-23,2.64697796016969E-23));
#17978=DIRECTION('center_axis',(-1.,5.29395592033937E-23,2.64697796016969E-23));
#17979=DIRECTION('ref_axis',(2.64697796016969E-23,-1.40129846432482E-45,
1.));
#17980=DIRECTION('',(-1.,5.29395592033937E-23,2.64697796016969E-23));
#17981=DIRECTION('center_axis',(2.64697796016969E-23,6.93889390390723E-15,
-1.));
#17982=DIRECTION('ref_axis',(-7.94093388050907E-23,1.,6.93889390390723E-15));
#17983=DIRECTION('center_axis',(0.707106781186548,4.99600361081321E-15,
-0.707106781186548));
#17984=DIRECTION('ref_axis',(-0.707106781186548,5.55111512312577E-17,-0.707106781186548));
#17985=DIRECTION('',(-1.39659253976245E-14,1.,-7.105427357601E-15));
#17986=DIRECTION('center_axis',(-0.70710678118654,-1.56975764458909E-14,
0.707106781186555));
#17987=DIRECTION('ref_axis',(0.707106781186555,4.51903224902127E-13,0.70710678118654));
#17988=DIRECTION('',(0.707106781186547,-5.55111512312578E-17,0.707106781186547));
#17989=DIRECTION('center_axis',(0.707106781186556,-6.72049359757844E-15,
-0.707106781186539));
#17990=DIRECTION('ref_axis',(0.707106781186539,9.95355220102466E-14,0.707106781186556));
#17991=DIRECTION('',(-6.95472852311166E-15,1.,-1.66533453693773E-16));
#17992=DIRECTION('center_axis',(-0.707106781186548,-8.69730586866937E-15,
0.707106781186547));
#17993=DIRECTION('ref_axis',(0.707106781186547,7.11593649168016E-14,0.707106781186548));
#17994=DIRECTION('',(0.707106781186548,4.88498130835069E-15,0.707106781186548));
#17995=DIRECTION('',(6.93919737993036E-15,-1.,1.66533453693773E-16));
#17996=DIRECTION('',(-0.707106781186547,5.55111512312578E-17,-0.707106781186547));
#17997=DIRECTION('center_axis',(-0.707106781186548,-9.88098491916389E-15,
-0.707106781186547));
#17998=DIRECTION('ref_axis',(-0.707106781186547,-5.55111512312579E-17,0.707106781186548));
#17999=DIRECTION('',(-0.707106781186547,-5.55111512312578E-17,0.707106781186548));
#18000=DIRECTION('',(-1.40096907165064E-14,1.,-1.66533453693773E-16));
#18001=DIRECTION('',(0.707106781186547,-4.82947015711943E-15,-0.707106781186548));
#18002=DIRECTION('center_axis',(0.70710678118653,-2.81071470146027E-14,
0.707106781186565));
#18003=DIRECTION('ref_axis',(0.707106781186565,3.61482073326878E-14,-0.70710678118653));
#18004=DIRECTION('',(1.39941595733251E-14,-1.,1.66533453693773E-16));
#18005=DIRECTION('center_axis',(-0.707106781186545,2.27462860225727E-15,
-0.70710678118655));
#18006=DIRECTION('ref_axis',(0.70710678118655,-1.72044670028397E-13,-0.707106781186545));
#18007=DIRECTION('',(0.707106781186547,5.55111512312579E-17,-0.707106781186548));
#18008=DIRECTION('center_axis',(0.707106781186553,2.76828881917404E-14,
0.707106781186542));
#18009=DIRECTION('ref_axis',(0.707106781186542,1.08542133667551E-13,-0.707106781186553));
#18010=DIRECTION('',(6.98296272528204E-15,-1.,7.105427357601E-15));
#18011=DIRECTION('center_axis',(-2.64697796016969E-23,1.,1.66533453693773E-16));
#18012=DIRECTION('ref_axis',(2.64697796016969E-23,-1.66533453693774E-16,
1.));
#18013=DIRECTION('',(1.,-2.64697796016969E-23,2.64697796016969E-23));
#18014=DIRECTION('',(1.,-2.64697796016969E-23,2.64697796016969E-23));
#18015=DIRECTION('center_axis',(-2.64697796016969E-23,-1.66533453693773E-16,
-1.));
#18016=DIRECTION('ref_axis',(-2.64697796016969E-23,1.,-1.66533453693774E-16));
#18017=DIRECTION('',(1.,-2.64697796016969E-23,2.64697796016969E-23));
#18018=DIRECTION('center_axis',(5.29395592033937E-23,-1.,6.88338275267597E-15));
#18019=DIRECTION('ref_axis',(-5.29395592033938E-23,-6.88338275267597E-15,
-1.));
#18020=DIRECTION('',(1.,-2.64697796016969E-23,2.64697796016969E-23));
#18021=DIRECTION('center_axis',(1.,-2.64697796016969E-23,2.64697796016969E-23));
#18022=DIRECTION('ref_axis',(2.64697796016969E-23,-7.00649232162408E-46,
-1.));
#18023=DIRECTION('',(1.,-2.64697796016969E-23,2.64697796016969E-23));
#18024=DIRECTION('center_axis',(2.64697796016969E-23,1.66533453693773E-16,
1.));
#18025=DIRECTION('ref_axis',(2.64697796016969E-23,-1.,1.66533453693774E-16));
#18026=DIRECTION('',(1.,-2.64697796016969E-23,2.64697796016969E-23));
#18027=DIRECTION('center_axis',(1.,-2.64697796016969E-23,2.64697796016969E-23));
#18028=DIRECTION('ref_axis',(2.64697796016969E-23,-7.00649232162408E-46,
-1.));
#18029=DIRECTION('',(1.,-2.64697796016969E-23,2.64697796016969E-23));
#18030=DIRECTION('center_axis',(2.64697796016969E-23,-1.,-1.66533453693773E-16));
#18031=DIRECTION('ref_axis',(-2.64697796016969E-23,1.66533453693774E-16,
-1.));
#18032=DIRECTION('',(1.,-2.64697796016969E-23,2.64697796016969E-23));
#18033=DIRECTION('center_axis',(1.,-2.64697796016969E-23,2.64697796016969E-23));
#18034=DIRECTION('ref_axis',(2.64697796016969E-23,1.68147671338624E-16,
-1.));
#18035=DIRECTION('',(1.,-2.64697796016969E-23,2.64697796016969E-23));
#18036=DIRECTION('center_axis',(5.29395592033938E-23,7.105427357601E-15,
1.));
#18037=DIRECTION('ref_axis',(5.29395592033938E-23,-1.,7.105427357601E-15));
#18038=DIRECTION('center_axis',(1.16649072924818E-39,0.,1.));
#18039=DIRECTION('ref_axis',(1.,0.,-1.16649072924818E-39));
#18040=DIRECTION('center_axis',(1.16649072924818E-39,0.,1.));
#18041=DIRECTION('ref_axis',(1.,0.,-1.16649072924818E-39));
#18042=DIRECTION('',(1.16649072924818E-39,0.,1.));
#18043=DIRECTION('center_axis',(1.16649072924818E-39,0.,1.));
#18044=DIRECTION('ref_axis',(1.,-5.87747175411142E-39,-1.16649072924818E-39));
#18045=DIRECTION('center_axis',(1.16649072924818E-39,0.,1.));
#18046=DIRECTION('ref_axis',(-0.667534157816547,0.744579175204459,7.78672406549494E-40));
#18047=DIRECTION('center_axis',(1.16649072924818E-39,0.,1.));
#18048=DIRECTION('ref_axis',(1.,0.,-1.16649072924818E-39));
#18049=DIRECTION('',(1.16649072924818E-39,0.,1.));
#18050=DIRECTION('center_axis',(1.16649072924818E-39,0.,1.));
#18051=DIRECTION('ref_axis',(1.,-5.87747175411143E-39,-1.16649072924818E-39));
#18052=DIRECTION('',(1.16649072924818E-39,0.,1.));
#18053=DIRECTION('center_axis',(1.16649072924818E-39,0.,1.));
#18054=DIRECTION('ref_axis',(-0.744579175204457,-0.66753415781655,8.68544705067255E-40));
#18055=DIRECTION('center_axis',(-1.16649072924818E-39,0.,-1.));
#18056=DIRECTION('ref_axis',(-1.,0.,1.16649072924818E-39));
#18057=DIRECTION('',(1.16649072924818E-39,0.,1.));
#18058=DIRECTION('center_axis',(-1.16649072924818E-39,0.,-1.));
#18059=DIRECTION('ref_axis',(-1.,0.,1.16649072924818E-39));
#18060=DIRECTION('center_axis',(-1.44079214459515E-16,1.,0.));
#18061=DIRECTION('ref_axis',(-1.,-1.44079214459515E-16,1.43985447997384E-40));
#18062=DIRECTION('',(-1.,-1.44079214459515E-16,1.4398546441885E-40));
#18063=DIRECTION('',(1.16649072924818E-39,0.,1.));
#18064=DIRECTION('',(-1.,-1.44079214459515E-16,1.4398546441885E-40));
#18065=DIRECTION('center_axis',(0.707106781186544,0.707106781186551,0.));
#18066=DIRECTION('ref_axis',(-0.707106781186551,0.707106781186544,0.));
#18067=DIRECTION('',(-0.707106781186551,0.707106781186544,0.));
#18068=DIRECTION('',(1.16649072924818E-39,0.,1.));
#18069=DIRECTION('',(-0.707106781186551,0.707106781186544,0.));
#18070=DIRECTION('center_axis',(1.,-5.87747175411144E-39,-1.16649072924818E-39));
#18071=DIRECTION('ref_axis',(-1.16649072924818E-39,0.,-1.));
#18072=DIRECTION('',(-5.87747175411144E-39,1.,0.));
#18073=DIRECTION('',(1.16649072924818E-39,0.,1.));
#18074=DIRECTION('',(-5.87747175411144E-39,1.,0.));
#18075=DIRECTION('center_axis',(5.87747175411144E-39,-1.,-6.85601631258903E-78));
#18076=DIRECTION('ref_axis',(-1.16649072924818E-39,0.,-1.));
#18077=DIRECTION('',(1.,-5.87747175411144E-39,1.16649072924818E-39));
#18078=DIRECTION('',(1.,-5.87747175411144E-39,1.16649072924818E-39));
#18079=DIRECTION('center_axis',(-1.16649072924818E-39,1.37120326251781E-77,
1.));
#18080=DIRECTION('ref_axis',(1.,-5.87747175411144E-39,1.16649072924818E-39));
#18081=DIRECTION('center_axis',(-1.16649072924818E-39,1.37120326251781E-77,
1.));
#18082=DIRECTION('ref_axis',(1.,-5.87747175411144E-39,1.16649072924818E-39));
#18083=DIRECTION('center_axis',(-1.16649072924818E-39,0.,-1.));
#18084=DIRECTION('ref_axis',(-1.,0.,1.16649072924818E-39));
#18085=DIRECTION('center_axis',(1.16649072924818E-39,0.,1.));
#18086=DIRECTION('ref_axis',(1.,0.,-1.16649072924818E-39));
#18087=DIRECTION('',(-1.16649072924818E-39,0.,-1.));
#18088=DIRECTION('center_axis',(1.16649072924818E-39,0.,1.));
#18089=DIRECTION('ref_axis',(1.,0.,-1.16649072924818E-39));
#18090=DIRECTION('center_axis',(1.16649072924818E-39,-1.37120326251781E-77,
-1.));
#18091=DIRECTION('ref_axis',(-1.,5.87747175411144E-39,-1.16649072924818E-39));
#18092=DIRECTION('',(-0.707106781186682,-0.707106781186413,0.));
#18093=DIRECTION('',(5.87747175411144E-39,-1.,0.));
#18094=DIRECTION('',(1.,2.39272203583008E-16,5.10666202579846E-39));
#18095=DIRECTION('center_axis',(1.16649072924818E-39,0.,1.));
#18096=DIRECTION('ref_axis',(-1.,0.,1.16649072924818E-39));
#18097=DIRECTION('',(1.91417762866406E-15,1.,0.));
#18098=DIRECTION('',(-1.,2.16502149887901E-16,-9.40207082428935E-39));
#18099=DIRECTION('center_axis',(1.16649072924818E-39,-1.37120326251781E-77,
-1.));
#18100=DIRECTION('ref_axis',(-1.,5.87747175411144E-39,-1.16649072924818E-39));
#18101=DIRECTION('',(-0.707106781186682,-0.707106781186413,0.));
#18102=DIRECTION('',(-1.,2.16502149887901E-16,-9.40207082428935E-39));
#18103=DIRECTION('',(1.91417762866406E-15,1.,0.));
#18104=DIRECTION('center_axis',(1.16649072924818E-39,0.,1.));
#18105=DIRECTION('ref_axis',(-1.,0.,1.16649072924818E-39));
#18106=DIRECTION('',(1.,2.39272203583008E-16,5.10666202579846E-39));
#18107=DIRECTION('',(5.87747175411144E-39,-1.,0.));
#18108=DIRECTION('center_axis',(0.707106781186413,-0.707106781186682,0.));
#18109=DIRECTION('ref_axis',(0.707106781186682,0.707106781186413,0.));
#18110=DIRECTION('',(-1.16649072924818E-39,0.,-1.));
#18111=DIRECTION('',(-1.16649072924818E-39,0.,-1.));
#18112=DIRECTION('center_axis',(1.,-5.87747175411144E-39,-1.16649072924818E-39));
#18113=DIRECTION('ref_axis',(-1.16649072924818E-39,0.,-1.));
#18114=DIRECTION('',(-1.16649072924818E-39,0.,-1.));
#18115=DIRECTION('center_axis',(-2.39272203583008E-16,1.,0.));
#18116=DIRECTION('ref_axis',(-1.,-2.39272203583008E-16,-5.10666202579846E-39));
#18117=DIRECTION('',(-1.16649072924818E-39,0.,-1.));
#18118=DIRECTION('center_axis',(-1.16649072924818E-39,0.,-1.));
#18119=DIRECTION('ref_axis',(-1.,0.,1.16649072924818E-39));
#18120=DIRECTION('',(-1.16649072924818E-39,0.,-1.));
#18121=DIRECTION('center_axis',(-1.,1.91417762866406E-15,9.67520394012289E-40));
#18122=DIRECTION('ref_axis',(-1.91417762866406E-15,-1.,-7.68355080092362E-71));
#18123=DIRECTION('',(-1.16649072924818E-39,0.,-1.));
#18124=DIRECTION('center_axis',(-2.16502149887901E-16,-1.,0.));
#18125=DIRECTION('ref_axis',(1.,-2.16502149887901E-16,9.40207082428935E-39));
#18126=DIRECTION('center_axis',(-1.16649072924818E-39,0.,-1.));
#18127=DIRECTION('ref_axis',(1.,-8.81620763116713E-39,-1.16649072924818E-39));
#18128=DIRECTION('center_axis',(1.16649072924818E-39,0.,1.));
#18129=DIRECTION('ref_axis',(1.,-8.81620763116713E-39,-1.16649072924818E-39));
#18130=DIRECTION('',(-1.16649072924818E-39,0.,-1.));
#18131=DIRECTION('center_axis',(1.16649072924818E-39,0.,1.));
#18132=DIRECTION('ref_axis',(1.,-8.81620763116713E-39,-1.16649072924818E-39));
#18133=DIRECTION('center_axis',(-1.16649072924818E-39,0.,-1.));
#18134=DIRECTION('ref_axis',(-0.66753415781655,0.744579175204457,7.78672406549497E-40));
#18135=DIRECTION('center_axis',(1.16649072924818E-39,0.,1.));
#18136=DIRECTION('ref_axis',(1.,-8.81620763116715E-39,-1.16649072924818E-39));
#18137=DIRECTION('',(-1.16649072924818E-39,0.,-1.));
#18138=DIRECTION('center_axis',(1.16649072924818E-39,0.,1.));
#18139=DIRECTION('ref_axis',(1.,-8.81620763116715E-39,-1.16649072924818E-39));
#18140=DIRECTION('',(-1.16649072924818E-39,0.,-1.));
#18141=DIRECTION('center_axis',(-1.16649072924818E-39,0.,-1.));
#18142=DIRECTION('ref_axis',(-0.744579175204457,-0.66753415781655,8.68544705067255E-40));
#18143=DIRECTION('center_axis',(-1.16649072924818E-39,0.,-1.));
#18144=DIRECTION('ref_axis',(-1.,0.,1.16649072924818E-39));
#18145=DIRECTION('center_axis',(-1.16649072924818E-39,0.,-1.));
#18146=DIRECTION('ref_axis',(-1.,0.,1.16649072924818E-39));
#18147=DIRECTION('',(-1.16649072924818E-39,0.,-1.));
#18148=DIRECTION('center_axis',(-1.44079214459515E-16,1.,0.));
#18149=DIRECTION('ref_axis',(-1.,-1.44079214459515E-16,1.43985447997384E-40));
#18150=DIRECTION('',(-1.,-1.44079214459515E-16,1.4398546441885E-40));
#18151=DIRECTION('',(-1.,-1.44079214459515E-16,1.4398546441885E-40));
#18152=DIRECTION('',(-1.16649072924818E-39,0.,-1.));
#18153=DIRECTION('center_axis',(0.707106781186544,0.707106781186551,0.));
#18154=DIRECTION('ref_axis',(-0.707106781186551,0.707106781186544,0.));
#18155=DIRECTION('',(-0.707106781186551,0.707106781186544,0.));
#18156=DIRECTION('',(-0.707106781186551,0.707106781186544,0.));
#18157=DIRECTION('',(-1.16649072924818E-39,0.,-1.));
#18158=DIRECTION('center_axis',(1.,-8.81620763116716E-39,-1.16649072924818E-39));
#18159=DIRECTION('ref_axis',(1.16649072924818E-39,0.,1.));
#18160=DIRECTION('',(-8.81620763116716E-39,1.,0.));
#18161=DIRECTION('',(-8.81620763116716E-39,1.,0.));
#18162=DIRECTION('',(-1.16649072924818E-39,0.,-1.));
#18163=DIRECTION('center_axis',(8.81620763116716E-39,-1.,-1.02840244688835E-77));
#18164=DIRECTION('ref_axis',(1.16649072924818E-39,0.,1.));
#18165=DIRECTION('',(1.,-8.81620763116716E-39,1.16649072924818E-39));
#18166=DIRECTION('',(1.,-8.81620763116716E-39,1.16649072924818E-39));
#18167=DIRECTION('center_axis',(1.16649072924818E-39,-2.05680489377671E-77,
-1.));
#18168=DIRECTION('ref_axis',(1.,-8.81620763116716E-39,1.16649072924818E-39));
#18169=DIRECTION('center_axis',(1.16649072924818E-39,-2.05680489377671E-77,
-1.));
#18170=DIRECTION('ref_axis',(1.,-8.81620763116716E-39,1.16649072924818E-39));
#18171=DIRECTION('center_axis',(1.16649072924818E-39,0.,1.));
#18172=DIRECTION('ref_axis',(-1.,0.,1.16649072924818E-39));
#18173=DIRECTION('center_axis',(1.16649072924818E-39,0.,1.));
#18174=DIRECTION('ref_axis',(1.,0.,-1.16649072924818E-39));
#18175=DIRECTION('',(1.16649072924818E-39,0.,1.));
#18176=DIRECTION('center_axis',(1.16649072924818E-39,0.,1.));
#18177=DIRECTION('ref_axis',(1.,0.,-1.16649072924818E-39));
#18178=DIRECTION('center_axis',(-1.16649072924818E-39,2.05680489377671E-77,
1.));
#18179=DIRECTION('ref_axis',(-1.,8.81620763116716E-39,-1.16649072924818E-39));
#18180=DIRECTION('',(-0.707106781186682,-0.707106781186413,0.));
#18181=DIRECTION('',(-1.,2.16502149887901E-16,-4.4666901348958E-38));
#18182=DIRECTION('',(1.91417762866406E-15,1.,0.));
#18183=DIRECTION('center_axis',(1.16649072924818E-39,0.,1.));
#18184=DIRECTION('ref_axis',(-1.,0.,1.16649072924818E-39));
#18185=DIRECTION('',(1.,2.39272203583008E-16,2.27390772881328E-38));
#18186=DIRECTION('',(2.35098870164458E-38,-1.,0.));
#18187=DIRECTION('center_axis',(-1.16649072924818E-39,2.05680489377671E-77,
1.));
#18188=DIRECTION('ref_axis',(-1.,8.81620763116716E-39,-1.16649072924818E-39));
#18189=DIRECTION('',(-0.707106781186682,-0.707106781186413,0.));
#18190=DIRECTION('',(2.35098870164458E-38,-1.,0.));
#18191=DIRECTION('',(1.,2.39272203583008E-16,2.27390772881328E-38));
#18192=DIRECTION('center_axis',(1.16649072924818E-39,0.,1.));
#18193=DIRECTION('ref_axis',(-1.,0.,1.16649072924818E-39));
#18194=DIRECTION('',(1.91417762866406E-15,1.,0.));
#18195=DIRECTION('',(-1.,2.16502149887901E-16,-4.4666901348958E-38));
#18196=DIRECTION('center_axis',(0.707106781186413,-0.707106781186682,0.));
#18197=DIRECTION('ref_axis',(0.707106781186682,0.707106781186413,0.));
#18198=DIRECTION('',(1.16649072924818E-39,0.,1.));
#18199=DIRECTION('',(1.16649072924818E-39,0.,1.));
#18200=DIRECTION('center_axis',(1.,-8.81620763116716E-39,-1.16649072924818E-39));
#18201=DIRECTION('ref_axis',(1.16649072924818E-39,0.,1.));
#18202=DIRECTION('',(1.16649072924818E-39,0.,1.));
#18203=DIRECTION('center_axis',(-2.39272203583008E-16,1.,0.));
#18204=DIRECTION('ref_axis',(-1.,-2.39272203583008E-16,-2.27390772881328E-38));
#18205=DIRECTION('',(1.16649072924818E-39,0.,1.));
#18206=DIRECTION('center_axis',(1.16649072924818E-39,0.,1.));
#18207=DIRECTION('ref_axis',(-1.,0.,1.16649072924818E-39));
#18208=DIRECTION('',(1.16649072924818E-39,0.,1.));
#18209=DIRECTION('center_axis',(-1.,1.91417762866406E-15,9.67520394012289E-40));
#18210=DIRECTION('ref_axis',(-1.91417762866406E-15,-1.,-7.68355080092362E-71));
#18211=DIRECTION('',(1.16649072924818E-39,0.,1.));
#18212=DIRECTION('center_axis',(-2.16502149887901E-16,-1.,0.));
#18213=DIRECTION('ref_axis',(1.,-2.16502149887901E-16,4.4666901348958E-38));
#18214=DIRECTION('center_axis',(7.04991620636974E-15,1.,0.));
#18215=DIRECTION('ref_axis',(-1.,7.04991620636974E-15,0.));
#18216=DIRECTION('center_axis',(-6.96737689119829E-15,-1.,0.));
#18217=DIRECTION('ref_axis',(1.,-6.96737689119829E-15,0.));
#18218=DIRECTION('',(7.04991620636974E-15,1.,0.));
#18219=DIRECTION('center_axis',(7.04991620636974E-15,1.,0.));
#18220=DIRECTION('ref_axis',(-1.,7.04991620636974E-15,0.));
#18221=DIRECTION('',(7.04991620636974E-15,1.,0.));
#18222=DIRECTION('center_axis',(7.04991620636974E-15,1.,0.));
#18223=DIRECTION('ref_axis',(-1.,7.04991620636974E-15,0.));
#18224=DIRECTION('center_axis',(-6.96737689119829E-15,-1.,0.));
#18225=DIRECTION('ref_axis',(1.,-6.96737689119829E-15,0.));
#18226=DIRECTION('',(7.04991620636974E-15,1.,0.));
#18227=DIRECTION('center_axis',(7.04991620636974E-15,1.,0.));
#18228=DIRECTION('ref_axis',(-1.,7.04991620636974E-15,0.));
#18229=DIRECTION('',(7.04991620636974E-15,1.,0.));
#18230=DIRECTION('center_axis',(-1.16649072924818E-39,0.,-1.));
#18231=DIRECTION('ref_axis',(-1.,0.,1.16649072924818E-39));
#18232=DIRECTION('center_axis',(-1.16649072924818E-39,0.,-1.));
#18233=DIRECTION('ref_axis',(1.,-7.10423911405687E-15,-1.16649072924818E-39));
#18234=DIRECTION('',(-1.16649072924818E-39,0.,-1.));
#18235=DIRECTION('center_axis',(1.16649072924818E-39,0.,1.));
#18236=DIRECTION('ref_axis',(-1.,0.,1.16649072924818E-39));
#18237=DIRECTION('',(-1.16649072924818E-39,0.,-1.));
#18238=DIRECTION('center_axis',(-1.16649072924818E-39,0.,-1.));
#18239=DIRECTION('ref_axis',(-1.,0.,1.16649072924818E-39));
#18240=DIRECTION('center_axis',(-1.16649072924818E-39,0.,-1.));
#18241=DIRECTION('ref_axis',(1.,-7.10423911405687E-15,-1.16649072924818E-39));
#18242=DIRECTION('',(-1.16649072924818E-39,0.,-1.));
#18243=DIRECTION('center_axis',(0.707106781186548,0.,-0.707106781186548));
#18244=DIRECTION('ref_axis',(0.707106781186548,2.39812798898023E-13,0.707106781186548));
#18245=DIRECTION('',(-1.16649072924818E-39,0.,-1.));
#18246=DIRECTION('center_axis',(1.,-5.87747175411144E-39,-1.16649072924818E-39));
#18247=DIRECTION('ref_axis',(-1.16649072924818E-39,0.,-1.));
#18248=DIRECTION('',(5.87747175411144E-39,-1.,0.));
#18249=DIRECTION('',(-1.16649072924818E-39,0.,-1.));
#18250=DIRECTION('',(-5.87747175411144E-39,1.,0.));
#18251=DIRECTION('center_axis',(1.,-5.87747175411144E-39,-1.16649072924818E-39));
#18252=DIRECTION('ref_axis',(-1.16649072924818E-39,0.,-1.));
#18253=DIRECTION('',(5.87747175411144E-39,-1.,0.));
#18254=DIRECTION('',(-1.16649072924818E-39,0.,-1.));
#18255=DIRECTION('',(5.87747175411144E-39,-1.,-6.98296267768627E-15));
#18256=DIRECTION('center_axis',(-0.707106781186547,4.93770026216453E-15,
-0.707106781186548));
#18257=DIRECTION('ref_axis',(-0.707106781186548,7.14278800091209E-32,0.707106781186547));
#18258=DIRECTION('',(-5.87747175411144E-39,1.,6.98296267768627E-15));
#18259=DIRECTION('center_axis',(0.707106781186551,-7.63665881151437E-15,
0.707106781186544));
#18260=DIRECTION('ref_axis',(0.707106781186544,-1.83022781783008E-13,-0.707106781186551));
#18261=DIRECTION('',(0.707106781186548,-4.92667944684876E-15,-0.707106781186548));
#18262=DIRECTION('center_axis',(-0.707106781186549,5.37639487806273E-15,
-0.707106781186546));
#18263=DIRECTION('ref_axis',(0.707106781186546,-2.782375660343E-13,-0.707106781186549));
#18264=DIRECTION('',(7.01119687164608E-15,1.,-2.82341939598112E-17));
#18265=DIRECTION('center_axis',(0.70710678118654,1.56975764458913E-14,0.707106781186555));
#18266=DIRECTION('ref_axis',(0.707106781186555,4.95830950211E-13,-0.70710678118654));
#18267=DIRECTION('',(0.707106781186548,0.,-0.707106781186548));
#18268=DIRECTION('',(-7.02672800395669E-15,-1.,4.37653262704196E-17));
#18269=DIRECTION('',(-0.707106781186548,4.93770026216453E-15,0.707106781186548));
#18270=DIRECTION('center_axis',(-0.707106781186547,-4.93770026216453E-15,
0.707106781186548));
#18271=DIRECTION('ref_axis',(0.707106781186548,1.39101446851167E-31,0.707106781186547));
#18272=DIRECTION('',(0.707106781186548,-4.93770026216453E-15,0.707106781186548));
#18273=DIRECTION('',(7.02672800395669E-15,1.,1.4009690681643E-14));
#18274=DIRECTION('',(-0.707106781186548,0.,-0.707106781186547));
#18275=DIRECTION('center_axis',(0.707106781186553,-4.56078234576569E-15,
-0.707106781186542));
#18276=DIRECTION('ref_axis',(0.707106781186542,3.97390229061337E-13,0.707106781186553));
#18277=DIRECTION('',(-7.01119687164608E-15,-1.,-1.39941595493323E-14));
#18278=DIRECTION('center_axis',(-0.707106781186546,-5.37639487806278E-15,
0.707106781186549));
#18279=DIRECTION('ref_axis',(0.707106781186549,-5.8955593170548E-14,0.707106781186546));
#18280=DIRECTION('',(-0.707106781186548,4.92667944684876E-15,-0.707106781186548));
#18281=DIRECTION('center_axis',(6.98296267768627E-15,1.,0.));
#18282=DIRECTION('ref_axis',(-1.,6.98296267768627E-15,-1.76663133728356E-39));
#18283=DIRECTION('',(1.,-7.04991620636974E-15,-8.33232385715269E-40));
#18284=DIRECTION('',(-1.,7.04991620636974E-15,8.33232385715269E-40));
#18285=DIRECTION('',(-1.16649072924818E-39,0.,-1.));
#18286=DIRECTION('',(-1.16649072924818E-39,0.,-1.));
#18287=DIRECTION('',(1.,-7.04991620636974E-15,-8.33232385715269E-40));
#18288=DIRECTION('',(-1.,7.04991620636974E-15,8.33232385715269E-40));
#18289=DIRECTION('center_axis',(-1.,7.02672800395669E-15,-2.86337824953972E-41));
#18290=DIRECTION('ref_axis',(-7.02672800395669E-15,-1.,-1.7794652584401E-71));
#18291=DIRECTION('',(-1.16649072924818E-39,0.,-1.));
#18292=DIRECTION('center_axis',(5.87747175411144E-39,-1.,-6.85601631258903E-78));
#18293=DIRECTION('ref_axis',(-1.16649072924818E-39,0.,-1.));
#18294=DIRECTION('',(-1.16649072924818E-39,0.,-1.));
#18295=DIRECTION('center_axis',(-1.16649072924818E-39,0.,-1.));
#18296=DIRECTION('ref_axis',(-1.,0.,1.16649072924818E-39));
#18297=DIRECTION('',(-1.16649072924818E-39,0.,-1.));
#18298=DIRECTION('center_axis',(1.,-7.01119687164608E-15,1.79234866735008E-39));
#18299=DIRECTION('ref_axis',(7.01119687164608E-15,1.,-4.81896270872514E-70));
#18300=DIRECTION('',(-1.16649072924818E-39,0.,-1.));
#18301=DIRECTION('center_axis',(-1.16649072924818E-39,0.,-1.));
#18302=DIRECTION('ref_axis',(-1.,0.,1.16649072924818E-39));
#18303=DIRECTION('',(-1.16649072924818E-39,0.,-1.));
#18304=DIRECTION('center_axis',(-6.96737689119829E-15,-1.,0.));
#18305=DIRECTION('ref_axis',(1.,-6.96737689119829E-15,-1.58475996252038E-40));
#18306=DIRECTION('',(-1.,6.96737689119829E-15,1.58475996252038E-40));
#18307=DIRECTION('',(1.,-6.96737689119829E-15,-1.58475996252038E-40));
#18308=DIRECTION('',(-1.,6.96737689119829E-15,1.58475996252038E-40));
#18309=DIRECTION('',(-1.16649072924818E-39,0.,-1.));
#18310=DIRECTION('',(1.,-6.96737689119829E-15,-1.58475996252038E-40));
#18311=DIRECTION('center_axis',(-1.16649072924818E-39,0.,-1.));
#18312=DIRECTION('ref_axis',(-1.,0.,1.16649072924818E-39));
#18313=DIRECTION('center_axis',(1.16649072924818E-39,0.,1.));
#18314=DIRECTION('ref_axis',(-1.,0.,1.16649072924818E-39));
#18315=DIRECTION('',(-1.16649072924818E-39,0.,-1.));
#18316=DIRECTION('center_axis',(1.,-5.87747175411144E-39,-1.16649072924818E-39));
#18317=DIRECTION('ref_axis',(-1.16649072924818E-39,0.,-1.));
#18318=DIRECTION('',(-5.87747175411144E-39,1.,0.));
#18319=DIRECTION('center_axis',(-1.16649072924818E-39,1.37120326251781E-77,
1.));
#18320=DIRECTION('ref_axis',(1.,-5.87747175411144E-39,1.16649072924818E-39));
#18321=DIRECTION('center_axis',(1.16649072924818E-39,-1.37120326251781E-77,
-1.));
#18322=DIRECTION('ref_axis',(-1.,5.87747175411144E-39,-1.16649072924818E-39));
#18323=DIRECTION('center_axis',(-1.16649072924818E-39,1.37120326251781E-77,
1.));
#18324=DIRECTION('ref_axis',(1.,-5.87747175411144E-39,1.16649072924818E-39));
#18325=DIRECTION('center_axis',(1.16649072924818E-39,-1.37120326251781E-77,
-1.));
#18326=DIRECTION('ref_axis',(-1.,5.87747175411144E-39,-1.16649072924818E-39));
#18327=DIRECTION('center_axis',(1.16649072924818E-39,0.,1.));
#18328=DIRECTION('ref_axis',(-1.,0.,1.16649072924818E-39));
#18329=DIRECTION('center_axis',(1.16649072924818E-39,0.,1.));
#18330=DIRECTION('ref_axis',(1.,0.,-1.16649072924818E-39));
#18331=DIRECTION('',(1.16649072924818E-39,0.,1.));
#18332=DIRECTION('center_axis',(1.16649072924818E-39,0.,1.));
#18333=DIRECTION('ref_axis',(1.,0.,-1.16649072924818E-39));
#18334=DIRECTION('center_axis',(-1.16649072924818E-39,1.37120326251781E-77,
1.));
#18335=DIRECTION('ref_axis',(-1.,5.87747175411144E-39,-1.16649072924818E-39));
#18336=DIRECTION('',(-0.707106781186682,-0.707106781186413,0.));
#18337=DIRECTION('',(-1.,2.16502149887901E-16,-9.40207082428935E-39));
#18338=DIRECTION('',(1.91417762866406E-15,1.,0.));
#18339=DIRECTION('center_axis',(1.16649072924818E-39,0.,1.));
#18340=DIRECTION('ref_axis',(-1.,0.,1.16649072924818E-39));
#18341=DIRECTION('',(1.,2.39272203583008E-16,5.10666202579846E-39));
#18342=DIRECTION('',(5.87747175411144E-39,-1.,0.));
#18343=DIRECTION('center_axis',(-1.16649072924818E-39,1.37120326251781E-77,
1.));
#18344=DIRECTION('ref_axis',(-1.,5.87747175411144E-39,-1.16649072924818E-39));
#18345=DIRECTION('',(-0.707106781186682,-0.707106781186413,0.));
#18346=DIRECTION('',(5.87747175411144E-39,-1.,0.));
#18347=DIRECTION('',(1.,2.39272203583008E-16,5.10666202579846E-39));
#18348=DIRECTION('center_axis',(1.16649072924818E-39,0.,1.));
#18349=DIRECTION('ref_axis',(-1.,0.,1.16649072924818E-39));
#18350=DIRECTION('',(1.91417762866406E-15,1.,0.));
#18351=DIRECTION('',(-1.,2.16502149887901E-16,-9.40207082428935E-39));
#18352=DIRECTION('center_axis',(0.707106781186413,-0.707106781186682,0.));
#18353=DIRECTION('ref_axis',(0.707106781186682,0.707106781186413,0.));
#18354=DIRECTION('',(1.16649072924818E-39,0.,1.));
#18355=DIRECTION('',(1.16649072924818E-39,0.,1.));
#18356=DIRECTION('center_axis',(1.,-5.87747175411144E-39,-1.16649072924818E-39));
#18357=DIRECTION('ref_axis',(1.16649072924818E-39,0.,1.));
#18358=DIRECTION('',(1.16649072924818E-39,0.,1.));
#18359=DIRECTION('center_axis',(-2.39272203583008E-16,1.,0.));
#18360=DIRECTION('ref_axis',(-1.,-2.39272203583008E-16,-5.10666202579846E-39));
#18361=DIRECTION('',(1.16649072924818E-39,0.,1.));
#18362=DIRECTION('center_axis',(1.16649072924818E-39,0.,1.));
#18363=DIRECTION('ref_axis',(-1.,0.,1.16649072924818E-39));
#18364=DIRECTION('',(1.16649072924818E-39,0.,1.));
#18365=DIRECTION('center_axis',(-1.,1.91417762866406E-15,9.67520394012289E-40));
#18366=DIRECTION('ref_axis',(-1.91417762866406E-15,-1.,-7.68355080092362E-71));
#18367=DIRECTION('',(1.16649072924818E-39,0.,1.));
#18368=DIRECTION('center_axis',(-2.16502149887901E-16,-1.,0.));
#18369=DIRECTION('ref_axis',(1.,-2.16502149887901E-16,9.40207082428935E-39));
#18370=DIRECTION('center_axis',(-1.16649072924818E-39,0.,-1.));
#18371=DIRECTION('ref_axis',(-1.,0.,1.16649072924818E-39));
#18372=DIRECTION('center_axis',(1.16649072924818E-39,0.,1.));
#18373=DIRECTION('ref_axis',(1.,0.,-1.16649072924818E-39));
#18374=DIRECTION('',(-1.16649072924818E-39,0.,-1.));
#18375=DIRECTION('center_axis',(1.16649072924818E-39,0.,1.));
#18376=DIRECTION('ref_axis',(1.,0.,-1.16649072924818E-39));
#18377=DIRECTION('center_axis',(1.16649072924818E-39,-1.37120326251781E-77,
-1.));
#18378=DIRECTION('ref_axis',(-1.,5.87747175411144E-39,-1.16649072924818E-39));
#18379=DIRECTION('',(-0.707106781186682,-0.707106781186413,0.));
#18380=DIRECTION('',(5.87747175411144E-39,-1.,0.));
#18381=DIRECTION('',(1.,2.39272203583008E-16,5.10666202579846E-39));
#18382=DIRECTION('center_axis',(1.16649072924818E-39,0.,1.));
#18383=DIRECTION('ref_axis',(-1.,0.,1.16649072924818E-39));
#18384=DIRECTION('',(1.91417762866406E-15,1.,0.));
#18385=DIRECTION('',(-1.,2.16502149887901E-16,-9.40207082428935E-39));
#18386=DIRECTION('center_axis',(1.16649072924818E-39,-1.37120326251781E-77,
-1.));
#18387=DIRECTION('ref_axis',(-1.,5.87747175411144E-39,-1.16649072924818E-39));
#18388=DIRECTION('',(-0.707106781186682,-0.707106781186413,0.));
#18389=DIRECTION('',(-1.,2.16502149887901E-16,-9.40207082428935E-39));
#18390=DIRECTION('',(1.91417762866406E-15,1.,0.));
#18391=DIRECTION('center_axis',(1.16649072924818E-39,0.,1.));
#18392=DIRECTION('ref_axis',(-1.,0.,1.16649072924818E-39));
#18393=DIRECTION('',(1.,2.39272203583008E-16,5.10666202579846E-39));
#18394=DIRECTION('',(5.87747175411144E-39,-1.,0.));
#18395=DIRECTION('center_axis',(0.707106781186413,-0.707106781186682,0.));
#18396=DIRECTION('ref_axis',(0.707106781186682,0.707106781186413,0.));
#18397=DIRECTION('',(-1.16649072924818E-39,0.,-1.));
#18398=DIRECTION('',(-1.16649072924818E-39,0.,-1.));
#18399=DIRECTION('center_axis',(1.,-5.87747175411144E-39,-1.16649072924818E-39));
#18400=DIRECTION('ref_axis',(-1.16649072924818E-39,0.,-1.));
#18401=DIRECTION('',(-1.16649072924818E-39,0.,-1.));
#18402=DIRECTION('center_axis',(-2.39272203583008E-16,1.,0.));
#18403=DIRECTION('ref_axis',(-1.,-2.39272203583008E-16,-5.10666202579846E-39));
#18404=DIRECTION('',(-1.16649072924818E-39,0.,-1.));
#18405=DIRECTION('center_axis',(-1.16649072924818E-39,0.,-1.));
#18406=DIRECTION('ref_axis',(-1.,0.,1.16649072924818E-39));
#18407=DIRECTION('',(-1.16649072924818E-39,0.,-1.));
#18408=DIRECTION('center_axis',(-1.,1.91417762866406E-15,9.67520394012289E-40));
#18409=DIRECTION('ref_axis',(-1.91417762866406E-15,-1.,-7.68355080092362E-71));
#18410=DIRECTION('',(-1.16649072924818E-39,0.,-1.));
#18411=DIRECTION('center_axis',(-2.16502149887901E-16,-1.,0.));
#18412=DIRECTION('ref_axis',(1.,-2.16502149887901E-16,9.40207082428935E-39));
#18413=DIRECTION('axis',(0.,0.,1.));
#18414=DIRECTION('refdir',(1.,0.,0.));
#18415=DIRECTION('center_axis',(1.,0.,-1.81014623580189E-15));
#18416=DIRECTION('ref_axis',(-1.81014623580189E-15,0.,-1.));
#18417=DIRECTION('',(-1.81014623580189E-15,0.,-1.));
#18418=DIRECTION('',(0.,1.,0.));
#18419=DIRECTION('',(-1.81014623580189E-15,0.,-1.));
#18420=DIRECTION('',(0.,1.,0.));
#18421=DIRECTION('center_axis',(0.,0.,1.));
#18422=DIRECTION('ref_axis',(1.,0.,0.));
#18423=DIRECTION('',(1.,0.,0.));
#18424=DIRECTION('',(0.,1.,0.));
#18425=DIRECTION('',(1.,0.,0.));
#18426=DIRECTION('center_axis',(0.,1.,0.));
#18427=DIRECTION('ref_axis',(0.,0.,1.));
#18428=DIRECTION('center_axis',(0.,-1.,0.));
#18429=DIRECTION('ref_axis',(0.,0.,1.));
#18430=DIRECTION('',(0.,1.,0.));
#18431=DIRECTION('center_axis',(0.,-1.,0.));
#18432=DIRECTION('ref_axis',(0.,0.,1.));
#18433=DIRECTION('center_axis',(-9.57088814332031E-16,0.,-1.));
#18434=DIRECTION('ref_axis',(-1.,0.,9.57088814332031E-16));
#18435=DIRECTION('',(-1.,0.,9.57088814332031E-16));
#18436=DIRECTION('',(0.,1.,0.));
#18437=DIRECTION('',(-1.,0.,9.57088814332031E-16));
#18438=DIRECTION('center_axis',(1.,0.,0.));
#18439=DIRECTION('ref_axis',(0.,0.,-1.));
#18440=DIRECTION('',(0.,0.,-1.));
#18441=DIRECTION('',(0.,1.,0.));
#18442=DIRECTION('',(0.,0.,-1.));
#18443=DIRECTION('center_axis',(0.,0.,1.));
#18444=DIRECTION('ref_axis',(1.,0.,0.));
#18445=DIRECTION('',(1.,0.,0.));
#18446=DIRECTION('',(0.,1.,0.));
#18447=DIRECTION('',(1.,0.,0.));
#18448=DIRECTION('center_axis',(0.,1.,0.));
#18449=DIRECTION('ref_axis',(0.,0.,1.));
#18450=DIRECTION('center_axis',(0.,-1.,0.));
#18451=DIRECTION('ref_axis',(0.,0.,1.));
#18452=DIRECTION('',(0.,1.,0.));
#18453=DIRECTION('center_axis',(0.,-1.,0.));
#18454=DIRECTION('ref_axis',(0.,0.,1.));
#18455=DIRECTION('center_axis',(0.,0.,-1.));
#18456=DIRECTION('ref_axis',(-1.,0.,0.));
#18457=DIRECTION('',(-1.,0.,0.));
#18458=DIRECTION('',(0.,1.,0.));
#18459=DIRECTION('',(-1.,0.,0.));
#18460=DIRECTION('center_axis',(1.,0.,1.81014623580188E-15));
#18461=DIRECTION('ref_axis',(1.81014623580188E-15,0.,-1.));
#18462=DIRECTION('',(1.81014623580188E-15,0.,-1.));
#18463=DIRECTION('',(0.,1.,0.));
#18464=DIRECTION('',(1.81014623580188E-15,0.,-1.));
#18465=DIRECTION('center_axis',(0.,0.,1.));
#18466=DIRECTION('ref_axis',(1.,0.,0.));
#18467=DIRECTION('',(1.,0.,0.));
#18468=DIRECTION('',(0.,1.,0.));
#18469=DIRECTION('',(1.,0.,0.));
#18470=DIRECTION('center_axis',(-1.,0.,0.));
#18471=DIRECTION('ref_axis',(0.,0.,1.));
#18472=DIRECTION('',(0.,0.,1.));
#18473=DIRECTION('',(0.,1.,0.));
#18474=DIRECTION('',(0.,0.,1.));
#18475=DIRECTION('center_axis',(0.,0.,-1.));
#18476=DIRECTION('ref_axis',(-1.,0.,0.));
#18477=DIRECTION('',(-1.,0.,0.));
#18478=DIRECTION('',(-1.,0.,0.));
#18479=DIRECTION('center_axis',(0.,1.,0.));
#18480=DIRECTION('ref_axis',(0.,0.,1.));
#18481=DIRECTION('center_axis',(0.,1.,0.));
#18482=DIRECTION('ref_axis',(0.,0.,1.));
#18483=DIRECTION('center_axis',(0.,0.,-1.));
#18484=DIRECTION('ref_axis',(-1.,0.,0.));
#18485=DIRECTION('center_axis',(0.,0.,1.));
#18486=DIRECTION('ref_axis',(1.,0.,0.));
#18487=DIRECTION('',(0.,0.,-1.));
#18488=DIRECTION('center_axis',(0.,0.,1.));
#18489=DIRECTION('ref_axis',(1.,0.,0.));
#18490=DIRECTION('center_axis',(0.,0.,-1.));
#18491=DIRECTION('ref_axis',(-1.,0.,0.));
#18492=DIRECTION('center_axis',(0.,0.,-1.));
#18493=DIRECTION('ref_axis',(1.,0.,0.));
#18494=DIRECTION('',(0.,0.,-1.));
#18495=DIRECTION('center_axis',(0.,0.,-1.));
#18496=DIRECTION('ref_axis',(1.,0.,0.));
#18497=DIRECTION('',(0.,0.,-1.));
#18498=DIRECTION('center_axis',(0.,0.,-1.));
#18499=DIRECTION('ref_axis',(-0.666666666666667,-0.74535599249993,0.));
#18500=DIRECTION('center_axis',(0.,0.,1.));
#18501=DIRECTION('ref_axis',(-1.,0.,0.));
#18502=DIRECTION('',(0.,0.,-1.));
#18503=DIRECTION('center_axis',(0.,0.,1.));
#18504=DIRECTION('ref_axis',(-1.,0.,0.));
#18505=DIRECTION('center_axis',(0.,0.,-1.));
#18506=DIRECTION('ref_axis',(-1.,0.,0.));
#18507=DIRECTION('',(1.,0.,0.));
#18508=DIRECTION('',(0.707106781186552,0.707106781186543,0.));
#18509=DIRECTION('',(-6.16790569236198E-15,1.,0.));
#18510=DIRECTION('',(-1.,0.,0.));
#18511=DIRECTION('center_axis',(0.,0.,-1.));
#18512=DIRECTION('ref_axis',(-1.,0.,0.));
#18513=DIRECTION('',(-1.,0.,0.));
#18514=DIRECTION('',(-6.16790569236198E-15,1.,0.));
#18515=DIRECTION('',(0.707106781186552,0.707106781186543,0.));
#18516=DIRECTION('',(1.,0.,0.));
#18517=DIRECTION('center_axis',(0.,1.,0.));
#18518=DIRECTION('ref_axis',(0.,0.,1.));
#18519=DIRECTION('',(0.,0.,-1.));
#18520=DIRECTION('center_axis',(-0.707106781186543,0.707106781186552,0.));
#18521=DIRECTION('ref_axis',(-0.707106781186552,-0.707106781186543,0.));
#18522=DIRECTION('',(0.,0.,-1.));
#18523=DIRECTION('center_axis',(-1.,-6.16790569236198E-15,0.));
#18524=DIRECTION('ref_axis',(6.16790569236198E-15,-1.,0.));
#18525=DIRECTION('',(0.,0.,-1.));
#18526=DIRECTION('center_axis',(0.,-1.,0.));
#18527=DIRECTION('ref_axis',(0.,0.,-1.));
#18528=DIRECTION('center_axis',(0.,0.,1.));
#18529=DIRECTION('ref_axis',(-1.,0.,0.));
#18530=DIRECTION('center_axis',(0.,0.,1.));
#18531=DIRECTION('ref_axis',(1.,0.,0.));
#18532=DIRECTION('',(0.,0.,1.));
#18533=DIRECTION('center_axis',(0.,0.,1.));
#18534=DIRECTION('ref_axis',(1.,0.,0.));
#18535=DIRECTION('center_axis',(0.,0.,1.));
#18536=DIRECTION('ref_axis',(-1.,0.,0.));
#18537=DIRECTION('center_axis',(0.,0.,-1.));
#18538=DIRECTION('ref_axis',(1.,0.,0.));
#18539=DIRECTION('',(0.,0.,1.));
#18540=DIRECTION('center_axis',(0.,0.,-1.));
#18541=DIRECTION('ref_axis',(1.,0.,0.));
#18542=DIRECTION('',(0.,0.,1.));
#18543=DIRECTION('center_axis',(0.,0.,1.));
#18544=DIRECTION('ref_axis',(-0.666666666666667,-0.74535599249993,0.));
#18545=DIRECTION('center_axis',(0.,0.,1.));
#18546=DIRECTION('ref_axis',(-1.,0.,0.));
#18547=DIRECTION('center_axis',(0.,0.,1.));
#18548=DIRECTION('ref_axis',(-1.,0.,0.));
#18549=DIRECTION('',(0.,0.,1.));
#18550=DIRECTION('center_axis',(0.,0.,1.));
#18551=DIRECTION('ref_axis',(-1.,0.,0.));
#18552=DIRECTION('',(-1.,0.,0.));
#18553=DIRECTION('',(-6.16790569236198E-15,1.,0.));
#18554=DIRECTION('',(0.707106781186552,0.707106781186543,0.));
#18555=DIRECTION('',(1.,0.,0.));
#18556=DIRECTION('center_axis',(0.,0.,1.));
#18557=DIRECTION('ref_axis',(-1.,0.,0.));
#18558=DIRECTION('',(1.,0.,0.));
#18559=DIRECTION('',(0.707106781186552,0.707106781186543,0.));
#18560=DIRECTION('',(-6.16790569236198E-15,1.,0.));
#18561=DIRECTION('',(-1.,0.,0.));
#18562=DIRECTION('center_axis',(0.,1.,0.));
#18563=DIRECTION('ref_axis',(0.,0.,-1.));
#18564=DIRECTION('',(0.,0.,1.));
#18565=DIRECTION('center_axis',(-0.707106781186543,0.707106781186552,0.));
#18566=DIRECTION('ref_axis',(-0.707106781186552,-0.707106781186543,0.));
#18567=DIRECTION('',(0.,0.,1.));
#18568=DIRECTION('center_axis',(-1.,-6.16790569236198E-15,0.));
#18569=DIRECTION('ref_axis',(6.16790569236198E-15,-1.,0.));
#18570=DIRECTION('',(0.,0.,1.));
#18571=DIRECTION('center_axis',(0.,-1.,0.));
#18572=DIRECTION('ref_axis',(0.,0.,1.));
#18573=DIRECTION('center_axis',(-1.,0.,0.));
#18574=DIRECTION('ref_axis',(0.,0.,1.));
#18575=DIRECTION('center_axis',(0.,4.44089209850063E-16,1.));
#18576=DIRECTION('ref_axis',(0.,-1.,4.44089209850063E-16));
#18577=DIRECTION('center_axis',(1.,0.,0.));
#18578=DIRECTION('ref_axis',(0.,0.,1.));
#18579=DIRECTION('center_axis',(0.,-1.,-1.60812264967664E-16));
#18580=DIRECTION('ref_axis',(0.,1.60812264967664E-16,-1.));
#18581=DIRECTION('center_axis',(0.,4.44089209850063E-16,1.));
#18582=DIRECTION('ref_axis',(0.,-1.,4.44089209850063E-16));
#18583=DIRECTION('center_axis',(-1.,0.,0.));
#18584=DIRECTION('ref_axis',(0.,0.,1.));
#18585=DIRECTION('center_axis',(0.,1.,-3.82856869892695E-16));
#18586=DIRECTION('ref_axis',(0.,3.82856869892695E-16,1.));
#18587=DIRECTION('center_axis',(1.,0.,0.));
#18588=DIRECTION('ref_axis',(0.,0.,1.));
#18589=DIRECTION('center_axis',(0.,4.44089209850063E-16,1.));
#18590=DIRECTION('ref_axis',(0.,-1.,4.44089209850063E-16));
#18591=DIRECTION('center_axis',(0.,4.44089209850063E-16,1.));
#18592=DIRECTION('ref_axis',(0.,-1.,4.44089209850063E-16));
#18593=DIRECTION('center_axis',(0.,1.,1.41610079671576E-16));
#18594=DIRECTION('ref_axis',(0.,-1.41610079671576E-16,1.));
#18595=DIRECTION('',(0.,-1.,-1.41610079671576E-16));
#18596=DIRECTION('center_axis',(0.,-1.,-1.60812264967664E-16));
#18597=DIRECTION('ref_axis',(0.,1.60812264967664E-16,-1.));
#18598=DIRECTION('center_axis',(0.,0.,-1.));
#18599=DIRECTION('ref_axis',(-1.,0.,0.));
#18600=DIRECTION('',(0.,0.,1.));
#18601=DIRECTION('center_axis',(0.,-1.,0.));
#18602=DIRECTION('ref_axis',(0.,0.,-1.));
#18603=DIRECTION('center_axis',(0.,1.,-3.82856869892695E-16));
#18604=DIRECTION('ref_axis',(0.,3.82856869892695E-16,1.));
#18605=DIRECTION('',(0.,1.,0.));
#18606=DIRECTION('center_axis',(0.,1.,-3.82856869892695E-16));
#18607=DIRECTION('ref_axis',(0.,3.82856869892695E-16,1.));
#18608=DIRECTION('center_axis',(0.,-1.,-1.60812264967664E-16));
#18609=DIRECTION('ref_axis',(0.,1.60812264967664E-16,-1.));
#18610=DIRECTION('axis',(0.,0.,1.));
#18611=DIRECTION('refdir',(1.,0.,0.));
#18612=DIRECTION('center_axis',(-1.,0.,0.));
#18613=DIRECTION('ref_axis',(0.,0.,1.));
#18614=DIRECTION('center_axis',(-1.,0.,0.));
#18615=DIRECTION('ref_axis',(0.,0.,1.));
#18616=DIRECTION('',(0.707106781186548,8.65956056235493E-17,0.707106781186547));
#18617=DIRECTION('center_axis',(-1.,0.,0.));
#18618=DIRECTION('ref_axis',(0.,0.,1.));
#18619=DIRECTION('center_axis',(-1.,0.,0.));
#18620=DIRECTION('ref_axis',(0.,0.,1.));
#18621=DIRECTION('center_axis',(-1.,0.,0.));
#18622=DIRECTION('ref_axis',(0.,0.,-1.));
#18623=DIRECTION('',(1.,0.,0.));
#18624=DIRECTION('center_axis',(0.,-0.866025403784438,0.500000000000001));
#18625=DIRECTION('ref_axis',(0.,-0.500000000000001,-0.866025403784438));
#18626=DIRECTION('',(-1.,0.,0.));
#18627=DIRECTION('',(0.,0.500000000000001,0.866025403784438));
#18628=DIRECTION('',(-1.,0.,0.));
#18629=DIRECTION('center_axis',(0.,-0.866025403784438,-0.500000000000001));
#18630=DIRECTION('ref_axis',(0.,0.500000000000001,-0.866025403784438));
#18631=DIRECTION('',(-1.,0.,0.));
#18632=DIRECTION('',(0.,-0.500000000000001,0.866025403784438));
#18633=DIRECTION('center_axis',(0.,-1.11386523624802E-16,-1.));
#18634=DIRECTION('ref_axis',(0.,1.,-1.11386523624802E-16));
#18635=DIRECTION('',(-1.,0.,0.));
#18636=DIRECTION('',(0.,-1.,1.11386523624802E-16));
#18637=DIRECTION('center_axis',(0.,0.866025403784438,-0.500000000000001));
#18638=DIRECTION('ref_axis',(0.,0.500000000000001,0.866025403784438));
#18639=DIRECTION('',(-1.,0.,0.));
#18640=DIRECTION('',(0.,-0.500000000000001,-0.866025403784438));
#18641=DIRECTION('center_axis',(0.,0.866025403784438,0.500000000000001));
#18642=DIRECTION('ref_axis',(0.,-0.500000000000001,0.866025403784438));
#18643=DIRECTION('',(-1.,0.,0.));
#18644=DIRECTION('',(0.,0.500000000000001,-0.866025403784438));
#18645=DIRECTION('center_axis',(0.,-2.22773047249605E-16,1.));
#18646=DIRECTION('ref_axis',(0.,-1.,-2.22773047249605E-16));
#18647=DIRECTION('',(0.,1.,2.22773047249605E-16));
#18648=DIRECTION('center_axis',(1.,0.,0.));
#18649=DIRECTION('ref_axis',(0.,0.,-1.));
#18650=DIRECTION('center_axis',(-1.,0.,0.));
#18651=DIRECTION('ref_axis',(0.,0.,1.));
#18652=DIRECTION('center_axis',(1.,0.,0.));
#18653=DIRECTION('ref_axis',(0.,0.,-1.));
#18654=DIRECTION('center_axis',(1.,0.,0.));
#18655=DIRECTION('ref_axis',(0.,0.,-1.));
#18656=DIRECTION('center_axis',(1.,0.,0.));
#18657=DIRECTION('ref_axis',(0.,0.,-1.));
#18658=DIRECTION('center_axis',(1.,0.,0.));
#18659=DIRECTION('ref_axis',(0.,0.,-1.));
#18660=DIRECTION('center_axis',(1.,0.,0.));
#18661=DIRECTION('ref_axis',(0.,0.,-1.));
#18662=DIRECTION('center_axis',(1.,0.,0.));
#18663=DIRECTION('ref_axis',(0.,0.,-1.));
#18664=DIRECTION('center_axis',(1.,0.,0.));
#18665=DIRECTION('ref_axis',(0.,0.,-1.));
#18666=DIRECTION('center_axis',(-1.,0.,0.));
#18667=DIRECTION('ref_axis',(0.,0.,1.));
#18668=DIRECTION('center_axis',(1.,0.,0.));
#18669=DIRECTION('ref_axis',(0.,0.,-1.));
#18670=DIRECTION('center_axis',(1.,0.,0.));
#18671=DIRECTION('ref_axis',(0.,0.,-1.));
#18672=DIRECTION('center_axis',(1.,0.,0.));
#18673=DIRECTION('ref_axis',(0.,0.,-1.));
#18674=DIRECTION('center_axis',(1.,0.,0.));
#18675=DIRECTION('ref_axis',(0.,0.,-1.));
#18676=DIRECTION('center_axis',(1.,0.,0.));
#18677=DIRECTION('ref_axis',(0.,0.,-1.));
#18678=DIRECTION('axis',(0.,0.,1.));
#18679=DIRECTION('refdir',(1.,0.,0.));
#18680=DIRECTION('center_axis',(-1.,0.,0.));
#18681=DIRECTION('ref_axis',(0.,0.,1.));
#18682=DIRECTION('center_axis',(-1.,0.,0.));
#18683=DIRECTION('ref_axis',(0.,0.,1.));
#18684=DIRECTION('',(0.707106781186551,8.65956056235489E-17,0.707106781186544));
#18685=DIRECTION('center_axis',(-1.,0.,0.));
#18686=DIRECTION('ref_axis',(0.,0.,1.));
#18687=DIRECTION('center_axis',(-1.,0.,0.));
#18688=DIRECTION('ref_axis',(0.,0.,1.));
#18689=DIRECTION('center_axis',(-1.,0.,0.));
#18690=DIRECTION('ref_axis',(0.,0.,-1.));
#18691=DIRECTION('',(1.,0.,0.));
#18692=DIRECTION('center_axis',(0.,-0.866025403784438,0.500000000000001));
#18693=DIRECTION('ref_axis',(0.,-0.500000000000001,-0.866025403784438));
#18694=DIRECTION('',(-1.,0.,0.));
#18695=DIRECTION('',(0.,0.500000000000001,0.866025403784438));
#18696=DIRECTION('',(-1.,0.,0.));
#18697=DIRECTION('center_axis',(0.,-0.866025403784438,-0.500000000000001));
#18698=DIRECTION('ref_axis',(0.,0.500000000000001,-0.866025403784438));
#18699=DIRECTION('',(-1.,0.,0.));
#18700=DIRECTION('',(0.,-0.500000000000001,0.866025403784438));
#18701=DIRECTION('center_axis',(0.,-2.22773047249605E-16,-1.));
#18702=DIRECTION('ref_axis',(0.,1.,-2.22773047249605E-16));
#18703=DIRECTION('',(-1.,0.,0.));
#18704=DIRECTION('',(0.,-1.,2.22773047249605E-16));
#18705=DIRECTION('center_axis',(0.,0.866025403784438,-0.500000000000002));
#18706=DIRECTION('ref_axis',(0.,0.500000000000002,0.866025403784438));
#18707=DIRECTION('',(-1.,0.,0.));
#18708=DIRECTION('',(0.,-0.500000000000002,-0.866025403784437));
#18709=DIRECTION('center_axis',(0.,0.866025403784439,0.5));
#18710=DIRECTION('ref_axis',(0.,-0.5,0.866025403784439));
#18711=DIRECTION('',(-1.,0.,0.));
#18712=DIRECTION('',(0.,0.5,-0.866025403784439));
#18713=DIRECTION('center_axis',(0.,-1.11386523624802E-16,1.));
#18714=DIRECTION('ref_axis',(0.,-1.,-1.11386523624802E-16));
#18715=DIRECTION('',(0.,1.,1.11386523624802E-16));
#18716=DIRECTION('center_axis',(1.,0.,0.));
#18717=DIRECTION('ref_axis',(0.,0.,-1.));
#18718=DIRECTION('center_axis',(-1.,0.,0.));
#18719=DIRECTION('ref_axis',(0.,0.,1.));
#18720=DIRECTION('center_axis',(1.,0.,0.));
#18721=DIRECTION('ref_axis',(0.,0.,-1.));
#18722=DIRECTION('center_axis',(1.,0.,0.));
#18723=DIRECTION('ref_axis',(0.,0.,-1.));
#18724=DIRECTION('center_axis',(1.,0.,0.));
#18725=DIRECTION('ref_axis',(0.,0.,-1.));
#18726=DIRECTION('center_axis',(1.,0.,0.));
#18727=DIRECTION('ref_axis',(0.,0.,-1.));
#18728=DIRECTION('center_axis',(1.,0.,0.));
#18729=DIRECTION('ref_axis',(0.,0.,-1.));
#18730=DIRECTION('center_axis',(1.,0.,0.));
#18731=DIRECTION('ref_axis',(0.,0.,-1.));
#18732=DIRECTION('center_axis',(1.,0.,0.));
#18733=DIRECTION('ref_axis',(0.,0.,-1.));
#18734=DIRECTION('center_axis',(-1.,0.,0.));
#18735=DIRECTION('ref_axis',(0.,0.,1.));
#18736=DIRECTION('center_axis',(1.,0.,0.));
#18737=DIRECTION('ref_axis',(0.,0.,-1.));
#18738=DIRECTION('center_axis',(1.,0.,0.));
#18739=DIRECTION('ref_axis',(0.,0.,-1.));
#18740=DIRECTION('center_axis',(1.,0.,0.));
#18741=DIRECTION('ref_axis',(0.,0.,-1.));
#18742=DIRECTION('center_axis',(1.,0.,0.));
#18743=DIRECTION('ref_axis',(0.,0.,-1.));
#18744=DIRECTION('center_axis',(1.,0.,0.));
#18745=DIRECTION('ref_axis',(0.,0.,-1.));
#18746=DIRECTION('axis',(0.,0.,1.));
#18747=DIRECTION('refdir',(1.,0.,0.));
#18748=DIRECTION('center_axis',(0.,0.,1.));
#18749=DIRECTION('ref_axis',(1.,0.,0.));
#18750=DIRECTION('center_axis',(0.,0.,1.));
#18751=DIRECTION('ref_axis',(-1.,0.,0.));
#18752=DIRECTION('',(0.,0.,1.));
#18753=DIRECTION('center_axis',(0.,0.,1.));
#18754=DIRECTION('ref_axis',(1.,0.,0.));
#18755=DIRECTION('center_axis',(0.,0.,1.));
#18756=DIRECTION('ref_axis',(1.,0.,0.));
#18757=DIRECTION('center_axis',(0.,0.,-1.));
#18758=DIRECTION('ref_axis',(-1.,0.,0.));
#18759=DIRECTION('center_axis',(0.,0.,1.));
#18760=DIRECTION('ref_axis',(-1.,0.,0.));
#18761=DIRECTION('',(0.819152044288988,-1.00317192905352E-16,-0.573576436351051));
#18762=DIRECTION('center_axis',(0.,0.,1.));
#18763=DIRECTION('ref_axis',(-1.,0.,0.));
#18764=DIRECTION('center_axis',(0.,0.,1.));
#18765=DIRECTION('ref_axis',(1.,0.,0.));
#18766=DIRECTION('center_axis',(0.,0.,-1.));
#18767=DIRECTION('ref_axis',(1.,0.,0.));
#18768=DIRECTION('',(-0.819152044288988,-1.00317192905352E-16,0.573576436351052));
#18769=DIRECTION('center_axis',(0.,0.,1.));
#18770=DIRECTION('ref_axis',(1.,0.,0.));
#18771=DIRECTION('center_axis',(0.,0.,1.));
#18772=DIRECTION('ref_axis',(1.,0.,0.));
#18773=DIRECTION('',(0.,0.,1.));
#18774=DIRECTION('center_axis',(-0.500000000000001,0.866025403784438,0.));
#18775=DIRECTION('ref_axis',(-0.866025403784438,-0.500000000000001,0.));
#18776=DIRECTION('',(0.,0.,1.));
#18777=DIRECTION('',(0.,0.,1.));
#18778=DIRECTION('center_axis',(0.500000000000001,0.866025403784438,0.));
#18779=DIRECTION('ref_axis',(-0.866025403784438,0.500000000000001,0.));
#18780=DIRECTION('',(0.,0.,1.));
#18781=DIRECTION('center_axis',(-1.,0.,0.));
#18782=DIRECTION('ref_axis',(0.,0.,1.));
#18783=DIRECTION('',(0.,0.,1.));
#18784=DIRECTION('center_axis',(0.500000000000001,-0.866025403784438,0.));
#18785=DIRECTION('ref_axis',(0.866025403784438,0.500000000000001,0.));
#18786=DIRECTION('',(0.,0.,1.));
#18787=DIRECTION('center_axis',(-0.500000000000001,-0.866025403784438,0.));
#18788=DIRECTION('ref_axis',(0.866025403784438,-0.500000000000001,0.));
#18789=DIRECTION('',(0.,0.,1.));
#18790=DIRECTION('center_axis',(-1.,1.26111394551748E-16,0.));
#18791=DIRECTION('ref_axis',(-1.26111394551748E-16,-1.,0.));
#18792=DIRECTION('center_axis',(0.,0.,-1.));
#18793=DIRECTION('ref_axis',(-1.,0.,0.));
#18794=DIRECTION('center_axis',(0.,0.,-1.));
#18795=DIRECTION('ref_axis',(-1.,0.,0.));
#18796=DIRECTION('center_axis',(0.,0.,-1.));
#18797=DIRECTION('ref_axis',(-1.,0.,0.));
#18798=DIRECTION('center_axis',(0.,0.,-1.));
#18799=DIRECTION('ref_axis',(-1.,0.,0.));
#18800=DIRECTION('center_axis',(0.,0.,-1.));
#18801=DIRECTION('ref_axis',(-1.,0.,0.));
#18802=DIRECTION('center_axis',(0.,0.,1.));
#18803=DIRECTION('ref_axis',(1.,0.,0.));
#18804=DIRECTION('center_axis',(0.,0.,-1.));
#18805=DIRECTION('ref_axis',(-1.,0.,0.));
#18806=DIRECTION('center_axis',(0.,0.,-1.));
#18807=DIRECTION('ref_axis',(-1.,0.,0.));
#18808=DIRECTION('center_axis',(0.,0.,1.));
#18809=DIRECTION('ref_axis',(-1.,0.,0.));
#18810=DIRECTION('center_axis',(0.,0.,1.));
#18811=DIRECTION('ref_axis',(-1.,-8.88178419700125E-16,0.));
#18812=DIRECTION('center_axis',(0.,0.,1.));
#18813=DIRECTION('ref_axis',(-1.,1.77635683940025E-15,0.));
#18814=DIRECTION('center_axis',(0.,0.,1.));
#18815=DIRECTION('ref_axis',(1.,0.,0.));
#18816=DIRECTION('center_axis',(0.,0.,1.));
#18817=DIRECTION('ref_axis',(-1.,1.77635683940025E-15,0.));
#18818=DIRECTION('center_axis',(0.,0.,1.));
#18819=DIRECTION('ref_axis',(-1.,0.,0.));
#18820=DIRECTION('center_axis',(0.,0.,1.));
#18821=DIRECTION('ref_axis',(1.,0.,0.));
#18822=DIRECTION('center_axis',(0.,0.,1.));
#18823=DIRECTION('ref_axis',(1.,0.,0.));
#18824=DIRECTION('center_axis',(0.,0.,1.));
#18825=DIRECTION('ref_axis',(1.,0.,0.));
#18826=DIRECTION('center_axis',(0.,0.,1.));
#18827=DIRECTION('ref_axis',(1.,0.,0.));
#18828=DIRECTION('center_axis',(0.,0.,1.));
#18829=DIRECTION('ref_axis',(1.,0.,0.));
#18830=DIRECTION('center_axis',(0.,0.,1.));
#18831=DIRECTION('ref_axis',(1.,0.,0.));
#18832=DIRECTION('center_axis',(0.,0.,-1.));
#18833=DIRECTION('ref_axis',(-1.,0.,0.));
#18834=DIRECTION('center_axis',(0.,0.,-1.));
#18835=DIRECTION('ref_axis',(-1.,0.,0.));
#18836=DIRECTION('center_axis',(0.,0.,-1.));
#18837=DIRECTION('ref_axis',(-1.,0.,0.));
#18838=DIRECTION('center_axis',(0.,0.,-1.));
#18839=DIRECTION('ref_axis',(-1.,0.,0.));
#18840=DIRECTION('center_axis',(0.,0.,-1.));
#18841=DIRECTION('ref_axis',(-1.,0.,0.));
#18842=DIRECTION('center_axis',(0.,0.,-1.));
#18843=DIRECTION('ref_axis',(-1.,0.,0.));
#18844=DIRECTION('axis',(0.,0.,1.));
#18845=DIRECTION('refdir',(1.,0.,0.));
#18846=DIRECTION('center_axis',(-8.74191357972136E-14,-1.,-3.36681878624147E-12));
#18847=DIRECTION('ref_axis',(-1.,8.79694822162854E-14,-1.3364594413628E-14));
#18848=DIRECTION('',(8.74191357972136E-14,1.,3.36681878624147E-12));
#18849=DIRECTION('center_axis',(2.81985569403837E-14,1.,-2.75774902090784E-13));
#18850=DIRECTION('ref_axis',(-3.32000459135762E-14,-2.76088836387462E-13,
-1.));
#18851=DIRECTION('center_axis',(-8.74191357972136E-14,-1.,-3.36681878624147E-12));
#18852=DIRECTION('ref_axis',(-1.,8.79694822162854E-14,-1.3364594413628E-14));
#18853=DIRECTION('',(8.74191357972136E-14,1.,3.36681878624147E-12));
#18854=DIRECTION('center_axis',(-8.74191357972136E-14,-1.,-3.36681878624147E-12));
#18855=DIRECTION('ref_axis',(-1.,8.79694822162854E-14,-1.3364594413628E-14));
#18856=DIRECTION('',(8.74191357972136E-14,1.,3.36681878624147E-12));
#18857=DIRECTION('center_axis',(-8.74191357972136E-14,-1.,-3.36681878624147E-12));
#18858=DIRECTION('ref_axis',(-1.,8.79694822162854E-14,-1.3364594413628E-14));
#18859=DIRECTION('',(8.74191357972136E-14,1.,3.36681878624147E-12));
#18860=DIRECTION('center_axis',(-8.74191357972136E-14,-1.,-3.36681878624147E-12));
#18861=DIRECTION('ref_axis',(-1.,8.79694822162854E-14,-1.3364594413628E-14));
#18862=DIRECTION('',(8.74191357972136E-14,1.,3.36681878624147E-12));
#18863=DIRECTION('center_axis',(-8.74191357972136E-14,-1.,-3.36681878624147E-12));
#18864=DIRECTION('ref_axis',(-1.,8.79694822162854E-14,-1.3364594413628E-14));
#18865=DIRECTION('',(8.74191357972136E-14,1.,3.36681878624147E-12));
#18866=DIRECTION('center_axis',(-8.74191357972136E-14,-1.,-3.36681878624147E-12));
#18867=DIRECTION('ref_axis',(-1.,8.79694822162854E-14,-1.3364594413628E-14));
#18868=DIRECTION('',(8.74191357972136E-14,1.,3.36681878624147E-12));
#18869=DIRECTION('center_axis',(-8.74191357972136E-14,-1.,-3.36681878624147E-12));
#18870=DIRECTION('ref_axis',(-1.,8.79694822162854E-14,-1.3364594413628E-14));
#18871=DIRECTION('',(8.74191357972136E-14,1.,3.36681878624147E-12));
#18872=DIRECTION('center_axis',(-8.74191357972136E-14,-1.,-3.36681878624147E-12));
#18873=DIRECTION('ref_axis',(-1.,8.79694822162854E-14,-1.3364594413628E-14));
#18874=DIRECTION('',(8.74191357972136E-14,1.,3.36681878624147E-12));
#18875=DIRECTION('center_axis',(-8.74191357972136E-14,-1.,-3.36681878624147E-12));
#18876=DIRECTION('ref_axis',(-1.,8.79694822162854E-14,-1.3364594413628E-14));
#18877=DIRECTION('',(8.74191357972136E-14,1.,3.36681878624147E-12));
#18878=DIRECTION('center_axis',(-8.74191357972136E-14,-1.,-3.36681878624147E-12));
#18879=DIRECTION('ref_axis',(-1.,8.79694822162854E-14,-1.3364594413628E-14));
#18880=DIRECTION('',(8.74191357972136E-14,1.,3.36681878624147E-12));
#18881=DIRECTION('center_axis',(-8.74191357972136E-14,-1.,-3.36681878624147E-12));
#18882=DIRECTION('ref_axis',(-1.,8.79694822162854E-14,-1.3364594413628E-14));
#18883=DIRECTION('',(8.74191357972136E-14,1.,3.36681878624147E-12));
#18884=DIRECTION('center_axis',(-8.74191357972136E-14,-1.,-3.36681878624147E-12));
#18885=DIRECTION('ref_axis',(-1.,8.79694822162854E-14,-1.3364594413628E-14));
#18886=DIRECTION('',(8.74191357972136E-14,1.,3.36681878624147E-12));
#18887=DIRECTION('center_axis',(-8.74191357972136E-14,-1.,-3.36681878624147E-12));
#18888=DIRECTION('ref_axis',(-1.,8.79694822162854E-14,-1.3364594413628E-14));
#18889=DIRECTION('',(8.74191357972136E-14,1.,3.36681878624147E-12));
#18890=DIRECTION('center_axis',(-8.74191357972136E-14,-1.,-3.36681878624147E-12));
#18891=DIRECTION('ref_axis',(-1.,8.79694822162854E-14,-1.3364594413628E-14));
#18892=DIRECTION('',(8.74191357972136E-14,1.,3.36681878624147E-12));
#18893=DIRECTION('center_axis',(-8.74191357972136E-14,-1.,-3.36681878624147E-12));
#18894=DIRECTION('ref_axis',(-1.,8.79694822162854E-14,-1.3364594413628E-14));
#18895=DIRECTION('',(8.74191357972136E-14,1.,3.36681878624147E-12));
#18896=DIRECTION('center_axis',(-8.74191357972136E-14,-1.,-3.36681878624147E-12));
#18897=DIRECTION('ref_axis',(-1.,8.79694822162854E-14,-1.3364594413628E-14));
#18898=DIRECTION('',(8.74191357972136E-14,1.,3.36681878624147E-12));
#18899=DIRECTION('center_axis',(-8.74191357972136E-14,-1.,-3.36681878624147E-12));
#18900=DIRECTION('ref_axis',(-1.,8.79694822162854E-14,-1.3364594413628E-14));
#18901=DIRECTION('',(8.74191357972136E-14,1.,3.36681878624147E-12));
#18902=DIRECTION('center_axis',(-8.74191357972136E-14,-1.,-3.36681878624147E-12));
#18903=DIRECTION('ref_axis',(-1.,8.79694822162854E-14,-1.3364594413628E-14));
#18904=DIRECTION('',(8.74191357972136E-14,1.,3.36681878624147E-12));
#18905=DIRECTION('center_axis',(-8.74191357972136E-14,-1.,-3.36681878624147E-12));
#18906=DIRECTION('ref_axis',(-1.,8.79694822162854E-14,-1.3364594413628E-14));
#18907=DIRECTION('',(8.74191357972136E-14,1.,3.36681878624147E-12));
#18908=DIRECTION('center_axis',(-8.74191357972136E-14,-1.,-3.36681878624147E-12));
#18909=DIRECTION('ref_axis',(-1.,8.79694822162854E-14,-1.3364594413628E-14));
#18910=DIRECTION('',(8.74191357972136E-14,1.,3.36681878624147E-12));
#18911=DIRECTION('center_axis',(-8.74191357972136E-14,-1.,-3.36681878624147E-12));
#18912=DIRECTION('ref_axis',(-1.,8.79694822162854E-14,-1.3364594413628E-14));
#18913=DIRECTION('',(8.74191357972136E-14,1.,3.36681878624147E-12));
#18914=DIRECTION('center_axis',(0.,1.,0.));
#18915=DIRECTION('ref_axis',(1.16649072924818E-39,0.,1.));
#18916=DIRECTION('',(0.,-1.,0.));
#18917=DIRECTION('',(0.,-1.,0.));
#18918=DIRECTION('',(0.,1.,0.));
#18919=DIRECTION('center_axis',(0.,1.,0.));
#18920=DIRECTION('ref_axis',(1.16649072924818E-39,0.,1.));
#18921=DIRECTION('',(0.,-1.,0.));
#18922=DIRECTION('center_axis',(0.,1.,0.));
#18923=DIRECTION('ref_axis',(1.16649072924818E-39,0.,1.));
#18924=DIRECTION('',(0.,-1.,0.));
#18925=DIRECTION('center_axis',(0.,1.,0.));
#18926=DIRECTION('ref_axis',(1.16649072924818E-39,0.,1.));
#18927=DIRECTION('',(0.,-1.,0.));
#18928=DIRECTION('center_axis',(0.,1.,0.));
#18929=DIRECTION('ref_axis',(1.16649072924818E-39,0.,1.));
#18930=DIRECTION('',(0.,-1.,0.));
#18931=DIRECTION('center_axis',(0.,1.,0.));
#18932=DIRECTION('ref_axis',(1.16649072924818E-39,0.,1.));
#18933=DIRECTION('',(0.,-1.,0.));
#18934=DIRECTION('center_axis',(0.,1.,0.));
#18935=DIRECTION('ref_axis',(1.16649072924818E-39,0.,1.));
#18936=DIRECTION('',(0.,-1.,0.));
#18937=DIRECTION('center_axis',(0.,1.,0.));
#18938=DIRECTION('ref_axis',(1.16649072924818E-39,0.,1.));
#18939=DIRECTION('',(0.,-1.,0.));
#18940=DIRECTION('center_axis',(0.,1.,0.));
#18941=DIRECTION('ref_axis',(1.16649072924818E-39,0.,1.));
#18942=DIRECTION('',(0.,-1.,0.));
#18943=DIRECTION('center_axis',(0.,1.,0.));
#18944=DIRECTION('ref_axis',(1.16649072924818E-39,0.,1.));
#18945=DIRECTION('',(0.,-1.,0.));
#18946=DIRECTION('center_axis',(0.,1.,0.));
#18947=DIRECTION('ref_axis',(1.16649072924818E-39,0.,1.));
#18948=DIRECTION('',(0.,-1.,0.));
#18949=DIRECTION('center_axis',(0.,1.,0.));
#18950=DIRECTION('ref_axis',(1.16649072924818E-39,0.,1.));
#18951=DIRECTION('',(0.,-1.,0.));
#18952=DIRECTION('center_axis',(0.,1.,0.));
#18953=DIRECTION('ref_axis',(1.16649072924818E-39,0.,1.));
#18954=DIRECTION('',(0.,-1.,0.));
#18955=DIRECTION('center_axis',(0.,1.,0.));
#18956=DIRECTION('ref_axis',(1.16649072924818E-39,0.,1.));
#18957=DIRECTION('',(0.,-1.,0.));
#18958=DIRECTION('center_axis',(0.,1.,0.));
#18959=DIRECTION('ref_axis',(1.16649072924818E-39,0.,1.));
#18960=DIRECTION('',(0.,-1.,0.));
#18961=DIRECTION('center_axis',(0.,1.,0.));
#18962=DIRECTION('ref_axis',(1.16649072924818E-39,0.,1.));
#18963=DIRECTION('',(0.,-1.,0.));
#18964=DIRECTION('center_axis',(0.,1.,0.));
#18965=DIRECTION('ref_axis',(1.16649072924818E-39,0.,1.));
#18966=DIRECTION('',(0.,-1.,0.));
#18967=DIRECTION('center_axis',(0.,1.,0.));
#18968=DIRECTION('ref_axis',(1.16649072924818E-39,0.,1.));
#18969=DIRECTION('',(0.,-1.,0.));
#18970=DIRECTION('center_axis',(0.,1.,0.));
#18971=DIRECTION('ref_axis',(1.16649072924818E-39,0.,1.));
#18972=DIRECTION('',(0.,-1.,0.));
#18973=DIRECTION('center_axis',(0.,1.,0.));
#18974=DIRECTION('ref_axis',(1.16649072924818E-39,0.,1.));
#18975=DIRECTION('',(0.,-1.,0.));
#18976=DIRECTION('center_axis',(0.,1.,0.));
#18977=DIRECTION('ref_axis',(1.16649072924818E-39,0.,1.));
#18978=DIRECTION('',(0.,-1.,0.));
#18979=DIRECTION('center_axis',(0.,-1.,0.));
#18980=DIRECTION('ref_axis',(1.16649072924818E-39,0.,1.));
#18981=DIRECTION('center_axis',(1.16649072924818E-39,0.,1.));
#18982=DIRECTION('ref_axis',(4.24488671257339E-14,-1.,0.));
#18983=DIRECTION('center_axis',(-1.16649072924818E-39,0.,-1.));
#18984=DIRECTION('ref_axis',(1.,-1.77635683940025E-15,-1.16649072924818E-39));
#18985=DIRECTION('center_axis',(0.910978406333114,-0.41245404979801,8.88703851014501E-13));
#18986=DIRECTION('ref_axis',(0.41245404979801,0.910978406333114,5.10955463663556E-29));
#18987=DIRECTION('center_axis',(1.16649072924818E-39,0.,1.));
#18988=DIRECTION('ref_axis',(1.,0.,-1.16649072924818E-39));
#18989=DIRECTION('center_axis',(0.910978406332847,0.4124540497986,2.48846969464753E-17));
#18990=DIRECTION('ref_axis',(-0.4124540497986,0.910978406332847,6.09192071292252E-33));
#18991=DIRECTION('center_axis',(1.16649072924818E-39,0.,1.));
#18992=DIRECTION('ref_axis',(-3.12699417093765E-14,-1.,0.));
#18993=DIRECTION('center_axis',(-1.16649072924818E-39,0.,-1.));
#18994=DIRECTION('ref_axis',(1.,1.77635683940025E-15,-1.16649072924818E-39));
#18995=DIRECTION('center_axis',(0.910978406332846,-0.412454049798602,0.));
#18996=DIRECTION('ref_axis',(0.412454049798602,0.910978406332846,0.));
#18997=DIRECTION('center_axis',(1.16649072924818E-39,0.,1.));
#18998=DIRECTION('ref_axis',(1.,0.,-1.16649072924818E-39));
#18999=DIRECTION('center_axis',(0.91097840633287,0.41245404979855,-2.46519032881566E-32));
#19000=DIRECTION('ref_axis',(-0.41245404979855,0.91097840633287,3.95416291609754E-48));
#19001=DIRECTION('center_axis',(1.16649072924818E-39,0.,1.));
#19002=DIRECTION('ref_axis',(1.,0.,-1.16649072924818E-39));
#19003=DIRECTION('center_axis',(1.16649072924818E-39,0.,1.));
#19004=DIRECTION('ref_axis',(1.,0.,-1.16649072924818E-39));
#19005=DIRECTION('',(1.16649072924818E-39,0.,1.));
#19006=DIRECTION('center_axis',(1.16649072924818E-39,0.,1.));
#19007=DIRECTION('ref_axis',(1.,0.,-1.16649072924818E-39));
#19008=DIRECTION('center_axis',(1.16649072924818E-39,0.,1.));
#19009=DIRECTION('ref_axis',(1.22508008559297E-14,-1.,-1.43194181381079E-53));
#19010=DIRECTION('center_axis',(0.,-1.,0.));
#19011=DIRECTION('ref_axis',(-1.16649072924818E-39,0.,-1.));
#19012=DIRECTION('center_axis',(0.,-1.,0.));
#19013=DIRECTION('ref_axis',(1.16649072924818E-39,0.,1.));
#19014=DIRECTION('',(8.65956056235491E-17,0.707106781186549,-0.707106781186546));
#19015=DIRECTION('center_axis',(0.,1.,0.));
#19016=DIRECTION('ref_axis',(1.16649072924818E-39,0.,1.));
#19017=DIRECTION('center_axis',(0.,1.,0.));
#19018=DIRECTION('ref_axis',(1.16649072924818E-39,0.,1.));
#19019=DIRECTION('center_axis',(-4.10522660630389E-39,0.,1.));
#19020=DIRECTION('ref_axis',(1.,0.,4.10522660630389E-39));
#19021=DIRECTION('center_axis',(-4.10522660630389E-39,0.,1.));
#19022=DIRECTION('ref_axis',(1.,0.,4.10522660630389E-39));
#19023=DIRECTION('center_axis',(0.,1.,0.));
#19024=DIRECTION('ref_axis',(1.16649072924818E-39,0.,1.));
#19025=DIRECTION('center_axis',(0.82190098044174,-4.46990853844586E-7,-0.569630387487103));
#19026=DIRECTION('ref_axis',(-0.56963038748716,-1.73470922087194E-18,-0.821900980441822));
#19027=DIRECTION('',(-0.493314502157547,-0.500000206354386,-0.711786903227801));
#19028=DIRECTION('',(0.49331421807717,-0.499999953061901,0.711787278040994));
#19029=DIRECTION('',(-3.67380332447989E-7,-0.9999999999999,2.54622298822739E-7));
#19030=DIRECTION('center_axis',(-8.74191357972136E-14,-1.,-3.36681878624147E-12));
#19031=DIRECTION('ref_axis',(-1.,8.79694822162854E-14,-1.3364594413628E-14));
#19032=DIRECTION('center_axis',(0.819989320180851,0.222433203783064,-0.527390732421558));
#19033=DIRECTION('ref_axis',(0.540942459779129,-2.5942501678163E-15,0.841059602649007));
#19034=DIRECTION('center_axis',(-0.81998932018085,-0.222433203783066,-0.527390732421559));
#19035=DIRECTION('ref_axis',(-0.540942459779129,3.37126789014689E-16,0.841059602649007));
#19036=DIRECTION('center_axis',(-0.81998932018085,0.222433203783066,0.527390732421559));
#19037=DIRECTION('ref_axis',(-0.54094245977913,-2.61757894185044E-15,-0.841059602649006));
#19038=DIRECTION('center_axis',(0.81998932018085,-0.222433203783066,0.527390732421559));
#19039=DIRECTION('ref_axis',(0.540942459779129,3.89141485738082E-16,-0.841059602649007));
#19040=DIRECTION('center_axis',(0.657353107750377,-0.75358270397543,2.46519032881566E-32));
#19041=DIRECTION('ref_axis',(0.75358270397543,0.657353107750377,-7.87577085156886E-48));
#19042=DIRECTION('center_axis',(0.657353107750364,0.753582703975442,0.));
#19043=DIRECTION('ref_axis',(-0.753582703975442,0.657353107750364,0.));
#19044=DIRECTION('center_axis',(0.657353107750348,-0.753582703975456,2.25915523143719E-14));
#19045=DIRECTION('ref_axis',(0.753582703975456,0.657353107750348,-8.1055088485032E-31));
#19046=DIRECTION('center_axis',(0.657353107749659,0.753582703976057,-1.03785565759232E-12));
#19047=DIRECTION('ref_axis',(-0.753582703976057,0.657353107749659,8.77882633459361E-29));
#19048=DIRECTION('axis',(0.,0.,1.));
#19049=DIRECTION('refdir',(1.,0.,0.));
#19050=DIRECTION('center_axis',(-7.2837465494537E-29,-1.,-1.47831161133771E-14));
#19051=DIRECTION('ref_axis',(-1.,0.,4.92707118958683E-15));
#19052=DIRECTION('',(-7.2837465494537E-29,-1.,-1.47831161133771E-14));
#19053=DIRECTION('center_axis',(6.93889390390723E-18,-1.,-7.50998708063543E-18));
#19054=DIRECTION('ref_axis',(-1.,0.,4.92707118958683E-15));
#19055=DIRECTION('center_axis',(-7.2837465494537E-29,-1.,-1.47831161133771E-14));
#19056=DIRECTION('ref_axis',(-1.,0.,4.92707118958683E-15));
#19057=DIRECTION('',(-7.2837465494537E-29,-1.,-1.47831161133771E-14));
#19058=DIRECTION('center_axis',(-7.2837465494537E-29,-1.,-1.47831161133771E-14));
#19059=DIRECTION('ref_axis',(-1.,0.,4.92707118958683E-15));
#19060=DIRECTION('',(-7.2837465494537E-29,-1.,-1.47831161133771E-14));
#19061=DIRECTION('center_axis',(-7.2837465494537E-29,-1.,-1.47831161133771E-14));
#19062=DIRECTION('ref_axis',(-1.,0.,4.92707118958683E-15));
#19063=DIRECTION('',(-7.2837465494537E-29,-1.,-1.47831161133771E-14));
#19064=DIRECTION('center_axis',(-7.2837465494537E-29,-1.,-1.47831161133771E-14));
#19065=DIRECTION('ref_axis',(-1.,0.,4.92707118958683E-15));
#19066=DIRECTION('',(-7.2837465494537E-29,-1.,-1.47831161133771E-14));
#19067=DIRECTION('center_axis',(-6.93889390390723E-18,1.,7.50998708063543E-18));
#19068=DIRECTION('ref_axis',(-1.,0.,4.92707118958683E-15));
#19069=DIRECTION('center_axis',(6.93889390390723E-18,-1.,7.50998708063543E-18));
#19070=DIRECTION('ref_axis',(3.2531186322964E-16,-7.50998708063542E-18,
-1.));
#19071=DIRECTION('',(6.93889390390723E-18,-1.,7.50998708063542E-18));
#19072=DIRECTION('center_axis',(-6.93889390390723E-18,1.,-7.50998708063543E-18));
#19073=DIRECTION('ref_axis',(-3.2531186322964E-16,7.50998708063542E-18,
1.));
#19074=DIRECTION('center_axis',(6.93889390390723E-18,-1.,7.50998708063543E-18));
#19075=DIRECTION('ref_axis',(3.2531186322964E-16,-7.50998708063542E-18,
-1.));
#19076=DIRECTION('',(6.93889390390723E-18,-1.,7.50998708063542E-18));
#19077=DIRECTION('center_axis',(-6.93889390390723E-18,1.,-7.50998708063543E-18));
#19078=DIRECTION('ref_axis',(-3.2531186322964E-16,7.50998708063542E-18,
1.));
#19079=DIRECTION('center_axis',(6.93889390390723E-18,-1.,7.50998708063543E-18));
#19080=DIRECTION('ref_axis',(3.2531186322964E-16,-7.50998708063542E-18,
-1.));
#19081=DIRECTION('',(6.93889390390723E-18,-1.,7.50998708063542E-18));
#19082=DIRECTION('center_axis',(6.93889390390723E-18,-1.,7.50998708063543E-18));
#19083=DIRECTION('ref_axis',(3.2531186322964E-16,-7.50998708063542E-18,
-1.));
#19084=DIRECTION('',(6.93889390390723E-18,-1.,7.50998708063542E-18));
#19085=DIRECTION('center_axis',(6.93889390390723E-18,-1.,7.50998708063543E-18));
#19086=DIRECTION('ref_axis',(3.2531186322964E-16,-7.50998708063542E-18,
-1.));
#19087=DIRECTION('',(6.93889390390723E-18,-1.,7.50998708063542E-18));
#19088=DIRECTION('center_axis',(6.93889390390723E-18,-1.,7.50998708063543E-18));
#19089=DIRECTION('ref_axis',(3.2531186322964E-16,-7.50998708063542E-18,
-1.));
#19090=DIRECTION('',(6.93889390390723E-18,-1.,7.50998708063542E-18));
#19091=DIRECTION('center_axis',(-6.93889390390723E-18,1.,-7.50998708063543E-18));
#19092=DIRECTION('ref_axis',(-3.2531186322964E-16,7.50998708063542E-18,
1.));
#19093=DIRECTION('center_axis',(-0.866025403784438,-0.500000000000002,2.85483331249634E-16));
#19094=DIRECTION('ref_axis',(0.500000000000002,-0.866025403784438,-1.56152092020898E-16));
#19095=DIRECTION('center_axis',(-0.866025403784438,-0.500000000000002,2.85483331249634E-16));
#19096=DIRECTION('ref_axis',(-0.500000000000002,0.866025403784438,-2.11601299807821E-14));
#19097=DIRECTION('',(0.96592582628907,-0.258819045102516,-2.25687796983236E-16));
#19098=DIRECTION('center_axis',(0.866025403784438,0.500000000000001,-2.85483331249634E-16));
#19099=DIRECTION('ref_axis',(-0.500000000000001,0.866025403784438,1.56152092020898E-16));
#19100=DIRECTION('center_axis',(-0.866025403784438,-0.500000000000001,2.85483331249634E-16));
#19101=DIRECTION('ref_axis',(0.500000000000001,-0.866025403784438,-1.56152092020897E-16));
#19102=DIRECTION('center_axis',(0.866025403784438,0.500000000000001,-2.85483331249634E-16));
#19103=DIRECTION('ref_axis',(-0.500000000000001,0.866025403784438,1.56152092020897E-16));
#19104=DIRECTION('',(0.866025403784438,0.500000000000001,-2.85483331249634E-16));
#19105=DIRECTION('center_axis',(0.866025403784438,0.500000000000001,-2.85483331249634E-16));
#19106=DIRECTION('ref_axis',(-0.500000000000001,0.866025403784438,1.56152092020897E-16));
#19107=DIRECTION('center_axis',(0.866025403784438,0.500000000000001,-2.85483331249634E-16));
#19108=DIRECTION('ref_axis',(-0.500000000000001,0.866025403784438,1.56152092020897E-16));
#19109=DIRECTION('',(-0.965925826289068,0.258819045102522,3.98879008230333E-16));
#19110=DIRECTION('center_axis',(-0.866025403784438,-0.500000000000001,2.85483331249634E-16));
#19111=DIRECTION('ref_axis',(0.500000000000001,-0.866025403784438,-1.56152092020896E-16));
#19112=DIRECTION('center_axis',(-0.866025403784166,-1.15935552460568E-13,
0.500000000000473));
#19113=DIRECTION('ref_axis',(-0.327326835368636,-0.75592894599349,-0.56694670953867));
#19114=DIRECTION('center_axis',(-0.86602540378437,-3.08582405011455E-14,
-0.500000000000119));
#19115=DIRECTION('ref_axis',(0.327326835357387,0.75592894601267,-0.566946709519592));
#19116=DIRECTION('center_axis',(-0.866025403784438,-0.500000000000001,2.85483331249634E-16));
#19117=DIRECTION('ref_axis',(0.500000000000001,-0.866025403784438,-1.56152092020896E-16));
#19118=DIRECTION('center_axis',(6.93889390390723E-18,-1.,7.50998708063543E-18));
#19119=DIRECTION('ref_axis',(3.2531186322964E-16,-7.50998708063542E-18,
-1.));
#19120=DIRECTION('center_axis',(6.93889390390723E-18,-1.,7.50998708063543E-18));
#19121=DIRECTION('ref_axis',(3.2531186322964E-16,-7.50998708063542E-18,
-1.));
#19122=DIRECTION('center_axis',(6.93889390390723E-18,-1.,7.50998708063543E-18));
#19123=DIRECTION('ref_axis',(3.2531186322964E-16,-7.50998708063542E-18,
-1.));
#19124=DIRECTION('center_axis',(-0.866025403784439,3.46944695195362E-18,
-0.5));
#19125=DIRECTION('ref_axis',(-0.5,-3.46944695195356E-18,0.866025403784439));
#19126=DIRECTION('center_axis',(-0.86602540378444,3.39006491526626E-15,
-0.499999999999998));
#19127=DIRECTION('ref_axis',(0.327326835353988,0.755928946018457,-0.566946709513838));
#19128=DIRECTION('',(0.5,1.73472347597681E-18,-0.866025403784439));
#19129=DIRECTION('',(6.93889390390723E-18,-1.,7.50998708063543E-18));
#19130=DIRECTION('',(0.5,1.73472347597681E-18,-0.866025403784439));
#19131=DIRECTION('',(6.93889390390723E-18,-1.,7.50998708063543E-18));
#19132=DIRECTION('center_axis',(-0.866025403784438,-1.73472347597681E-18,
0.5));
#19133=DIRECTION('ref_axis',(0.5,-8.67361737988409E-18,0.866025403784438));
#19134=DIRECTION('center_axis',(-0.866025403784443,6.78860499282057E-15,
0.499999999999992));
#19135=DIRECTION('ref_axis',(-0.327326835353985,-0.755928946018458,-0.566946709513837));
#19136=DIRECTION('',(-0.5,1.04083408558608E-17,-0.866025403784438));
#19137=DIRECTION('',(6.93889390390723E-18,-1.,7.50998708063543E-18));
#19138=DIRECTION('',(-0.5,1.04083408558608E-17,-0.866025403784438));
#19139=DIRECTION('center_axis',(-6.93889390390723E-18,1.,7.50998708063543E-18));
#19140=DIRECTION('ref_axis',(-3.2531186322964E-16,-7.50998708063543E-18,
1.));
#19141=DIRECTION('center_axis',(6.93889390390723E-18,-1.,7.50998708063543E-18));
#19142=DIRECTION('ref_axis',(3.2531186322964E-16,-7.50998708063542E-18,
-1.));
#19143=DIRECTION('center_axis',(6.93889390390723E-18,-1.,7.50998708063543E-18));
#19144=DIRECTION('ref_axis',(3.2531186322964E-16,-7.50998708063542E-18,
-1.));
#19145=DIRECTION('',(-1.,6.93889390390723E-18,3.2531186322964E-16));
#19146=DIRECTION('center_axis',(6.93889390390723E-18,-1.,7.50998708063543E-18));
#19147=DIRECTION('ref_axis',(3.2531186322964E-16,-7.50998708063542E-18,
-1.));
#19148=DIRECTION('',(-0.5,-3.46944695195356E-18,0.866025403784438));
#19149=DIRECTION('center_axis',(6.93889390390723E-18,-1.,7.50998708063543E-18));
#19150=DIRECTION('ref_axis',(3.2531186322964E-16,-7.50998708063542E-18,
-1.));
#19151=DIRECTION('',(0.5,-8.67361737988404E-18,0.866025403784438));
#19152=DIRECTION('center_axis',(6.93889390390723E-18,-1.,7.50998708063543E-18));
#19153=DIRECTION('ref_axis',(3.2531186322964E-16,-7.50998708063542E-18,
-1.));
#19154=DIRECTION('',(1.,-6.93889390390723E-18,-3.2531186322964E-16));
#19155=DIRECTION('center_axis',(6.93889390390723E-18,-1.,7.50998708063543E-18));
#19156=DIRECTION('ref_axis',(3.2531186322964E-16,-7.50998708063542E-18,
-1.));
#19157=DIRECTION('center_axis',(-6.93889390390723E-18,1.,7.50998708063543E-18));
#19158=DIRECTION('ref_axis',(-3.2531186322964E-16,-7.50998708063543E-18,
1.));
#19159=DIRECTION('center_axis',(6.93889390390723E-18,-1.,7.50998708063543E-18));
#19160=DIRECTION('ref_axis',(3.2531186322964E-16,-7.50998708063542E-18,
-1.));
#19161=DIRECTION('',(1.,-6.93889390390723E-18,-3.2531186322964E-16));
#19162=DIRECTION('center_axis',(6.93889390390723E-18,-1.,7.50998708063543E-18));
#19163=DIRECTION('ref_axis',(3.2531186322964E-16,-7.50998708063542E-18,
-1.));
#19164=DIRECTION('',(0.5,-8.67361737988404E-18,0.866025403784438));
#19165=DIRECTION('center_axis',(6.93889390390723E-18,-1.,7.50998708063543E-18));
#19166=DIRECTION('ref_axis',(3.2531186322964E-16,-7.50998708063542E-18,
-1.));
#19167=DIRECTION('',(-0.5,-3.46944695195356E-18,0.866025403784438));
#19168=DIRECTION('center_axis',(6.93889390390723E-18,-1.,7.50998708063543E-18));
#19169=DIRECTION('ref_axis',(3.2531186322964E-16,-7.50998708063542E-18,
-1.));
#19170=DIRECTION('',(-1.,6.93889390390723E-18,1.99119960773767E-16));
#19171=DIRECTION('center_axis',(6.93889390390723E-18,-1.,7.50998708063543E-18));
#19172=DIRECTION('ref_axis',(3.2531186322964E-16,-7.50998708063542E-18,
-1.));
#19173=DIRECTION('center_axis',(6.93889390390723E-18,-1.,7.50998708063543E-18));
#19174=DIRECTION('ref_axis',(3.2531186322964E-16,-7.50998708063542E-18,
-1.));
#19175=DIRECTION('center_axis',(1.99119960773767E-16,-7.50998708063543E-18,
1.));
#19176=DIRECTION('ref_axis',(1.,-6.93889390390723E-18,-1.99119960773767E-16));
#19177=DIRECTION('',(6.93889390390723E-18,-1.,7.50998708063543E-18));
#19178=DIRECTION('center_axis',(0.866025403784438,-6.93889390390723E-18,
0.5));
#19179=DIRECTION('ref_axis',(0.5,3.46944695195361E-18,-0.866025403784438));
#19180=DIRECTION('',(6.93889390390723E-18,-1.,7.50998708063543E-18));
#19181=DIRECTION('center_axis',(0.866025403784439,3.46944695195364E-18,
-0.5));
#19182=DIRECTION('ref_axis',(-0.5,1.04083408558609E-17,-0.866025403784439));
#19183=DIRECTION('',(6.93889390390723E-18,-1.,7.50998708063543E-18));
#19184=DIRECTION('center_axis',(-3.2531186322964E-16,7.50998708063543E-18,
-1.));
#19185=DIRECTION('ref_axis',(-1.,6.93889390390723E-18,3.2531186322964E-16));
#19186=DIRECTION('center_axis',(-6.93889390390723E-18,1.,-7.50998708063543E-18));
#19187=DIRECTION('ref_axis',(-3.2531186322964E-16,7.50998708063542E-18,
1.));
#19188=DIRECTION('center_axis',(-6.93889390390723E-18,1.,-7.50998708063543E-18));
#19189=DIRECTION('ref_axis',(-3.2531186322964E-16,7.50998708063542E-18,
1.));
#19190=DIRECTION('center_axis',(6.93889390390723E-18,-1.,7.50998708063543E-18));
#19191=DIRECTION('ref_axis',(3.2531186322964E-16,-7.50998708063542E-18,
-1.));
#19192=DIRECTION('center_axis',(6.93889390390723E-18,-1.,7.50998708063543E-18));
#19193=DIRECTION('ref_axis',(3.2531186322964E-16,-7.50998708063542E-18,
-1.));
#19194=DIRECTION('center_axis',(-6.93889390390723E-18,1.,-7.50998708063543E-18));
#19195=DIRECTION('ref_axis',(-3.2531186322964E-16,7.50998708063542E-18,
1.));
#19196=DIRECTION('center_axis',(6.93889390390723E-18,-1.,7.50998708063543E-18));
#19197=DIRECTION('ref_axis',(3.2531186322964E-16,-7.50998708063542E-18,
-1.));
#19198=DIRECTION('center_axis',(-6.93889390390723E-18,1.,-7.50998708063543E-18));
#19199=DIRECTION('ref_axis',(-3.2531186322964E-16,7.50998708063542E-18,
1.));
#19200=DIRECTION('center_axis',(6.93889390390723E-18,-1.,7.50998708063543E-18));
#19201=DIRECTION('ref_axis',(3.2531186322964E-16,-7.50998708063542E-18,
-1.));
#19202=DIRECTION('center_axis',(-6.93889390390723E-18,1.,-7.50998708063543E-18));
#19203=DIRECTION('ref_axis',(-3.2531186322964E-16,7.50998708063542E-18,
1.));
#19204=DIRECTION('center_axis',(6.93889390390723E-18,-1.,7.50998708063543E-18));
#19205=DIRECTION('ref_axis',(3.2531186322964E-16,-7.50998708063542E-18,
-1.));
#19206=DIRECTION('center_axis',(-6.93889390390723E-18,1.,-7.50998708063543E-18));
#19207=DIRECTION('ref_axis',(-3.2531186322964E-16,7.50998708063542E-18,
1.));
#19208=DIRECTION('center_axis',(6.93889390390723E-18,-1.,7.50998708063543E-18));
#19209=DIRECTION('ref_axis',(3.2531186322964E-16,-7.50998708063542E-18,
-1.));
#19210=DIRECTION('center_axis',(-7.2837465494537E-29,-1.,-1.47831161133771E-14));
#19211=DIRECTION('ref_axis',(-1.,0.,4.92707118958683E-15));
#19212=DIRECTION('center_axis',(0.866025403784438,0.500000000000001,-2.85483331249634E-16));
#19213=DIRECTION('ref_axis',(0.500000000000001,-0.866025403784438,4.40720468639446E-15));
#19214=DIRECTION('center_axis',(0.866025403784438,0.500000000000001,-2.85483331249634E-16));
#19215=DIRECTION('ref_axis',(-0.500000000000001,0.866025403784438,1.56152092020897E-16));
#19216=DIRECTION('axis',(0.,0.,1.));
#19217=DIRECTION('refdir',(1.,0.,0.));
#19218=DIRECTION('center_axis',(-1.,0.,0.));
#19219=DIRECTION('ref_axis',(0.,0.,1.));
#19220=DIRECTION('center_axis',(-1.,0.,0.));
#19221=DIRECTION('ref_axis',(0.,0.,1.));
#19222=DIRECTION('',(1.,0.,0.));
#19223=DIRECTION('center_axis',(-1.,0.,0.));
#19224=DIRECTION('ref_axis',(0.,0.,1.));
#19225=DIRECTION('center_axis',(-1.,0.,0.));
#19226=DIRECTION('ref_axis',(0.,0.,1.));
#19227=DIRECTION('center_axis',(-1.,0.,0.));
#19228=DIRECTION('ref_axis',(0.,0.,1.));
#19229=DIRECTION('',(-1.,0.,0.));
#19230=DIRECTION('center_axis',(-1.,0.,0.));
#19231=DIRECTION('ref_axis',(0.,0.,1.));
#19232=DIRECTION('center_axis',(-1.,0.,0.));
#19233=DIRECTION('ref_axis',(0.,0.,1.));
#19234=DIRECTION('center_axis',(1.,0.,0.));
#19235=DIRECTION('ref_axis',(0.,0.,-1.));
#19236=DIRECTION('',(1.16649072924818E-39,0.,1.));
#19237=DIRECTION('',(1.,-2.93873587705572E-39,-1.16649072924818E-39));
#19238=DIRECTION('',(1.16649072924818E-39,0.,1.));
#19239=DIRECTION('',(1.,-2.93873587705572E-39,-1.16649072924818E-39));
#19240=DIRECTION('',(-1.,2.93873587705572E-39,-1.16649072924818E-39));
#19241=DIRECTION('',(1.16649072924818E-39,-6.85601631258903E-78,-1.));
#19242=DIRECTION('',(-1.,1.44415729375069E-15,-2.43230792576604E-39));
#19243=DIRECTION('',(2.43230792576604E-39,-5.19723132637897E-54,-1.));
#19244=DIRECTION('',(1.,-2.93873587705572E-39,1.16649072924818E-39));
#19245=DIRECTION('',(1.16649072924818E-39,-6.85601631258903E-78,-1.));
#19246=DIRECTION('',(-1.16649072924818E-39,-3.12598350966825E-71,-1.));
#19247=DIRECTION('',(1.,-4.04190569902596E-16,-1.16649072924818E-39));
#19248=DIRECTION('',(1.16649072924818E-39,0.,1.));
#19249=DIRECTION('',(1.,-2.93873587705572E-39,-1.16649072924818E-39));
#19250=DIRECTION('',(1.11022302462516E-16,-8.10428829229619E-19,-1.));
#19251=DIRECTION('',(-1.,-4.85703854817883E-18,-1.11022302462516E-16));
#19252=DIRECTION('',(1.,-2.93873587705572E-39,1.16649072924818E-39));
#19253=DIRECTION('',(-1.16649072924818E-39,6.85601631258903E-78,1.));
#19254=DIRECTION('',(-1.,2.93873587705572E-39,-1.16649072924818E-39));
#19255=DIRECTION('',(1.16649072924818E-39,-6.85601631258903E-78,-1.));
#19256=DIRECTION('',(1.,-2.93873587705572E-39,1.16649072924818E-39));
#19257=DIRECTION('',(-1.16649072924818E-39,6.85601631258903E-78,1.));
#19258=DIRECTION('',(1.,-1.44415729375069E-15,2.43230792576604E-39));
#19259=DIRECTION('',(-2.43230792576604E-39,5.19723132637897E-54,1.));
#19260=DIRECTION('',(-1.,2.93873587705572E-39,-1.16649072924818E-39));
#19261=DIRECTION('',(-1.16649072924818E-39,6.85601631258903E-78,1.));
#19262=DIRECTION('',(1.16649072924818E-39,0.,1.));
#19263=DIRECTION('',(1.,-2.93873587705572E-39,-1.16649072924818E-39));
#19264=DIRECTION('',(-1.16649072924818E-39,0.,-1.));
#19265=DIRECTION('',(1.,-2.93873587705572E-39,-1.16649072924818E-39));
#19266=DIRECTION('',(1.16649072924818E-39,0.,1.));
#19267=DIRECTION('',(1.,-2.93873587705572E-39,-1.16649072924818E-39));
#19268=DIRECTION('',(1.16649072924818E-39,-2.08157947664722E-57,1.));
#19269=DIRECTION('',(0.999846167219613,0.0175397233800904,-1.166311284736E-39));
#19270=DIRECTION('',(-0.447826234236897,-1.56911486851057E-16,0.894120609274386));
#19271=DIRECTION('',(-7.7186648647211E-17,1.,1.36833084244975E-16));
#19272=DIRECTION('',(-1.11022302462516E-16,-2.22044604925031E-16,-1.));
#19273=DIRECTION('',(-0.999846167219613,-0.01753972338009,1.14899824541469E-16));
#19274=DIRECTION('',(-0.447757343882154,-0.00785474827086252,0.894120609274387));
#19275=DIRECTION('',(-0.0175397233800901,0.999846167219613,-8.23527328298367E-17));
#19276=DIRECTION('axis',(0.,0.,1.));
#19277=DIRECTION('refdir',(1.,0.,0.));
#19278=DIRECTION('center_axis',(-1.,0.,0.));
#19279=DIRECTION('ref_axis',(0.,0.,1.));
#19280=DIRECTION('',(0.,1.,0.));
#19281=DIRECTION('',(0.,0.,-1.));
#19282=DIRECTION('',(0.,1.,0.));
#19283=DIRECTION('',(0.,0.,-1.));
#19284=DIRECTION('center_axis',(0.,-1.,0.));
#19285=DIRECTION('ref_axis',(0.,0.,-1.));
#19286=DIRECTION('',(-1.,0.,0.));
#19287=DIRECTION('',(0.,0.,-1.));
#19288=DIRECTION('',(-1.,0.,0.));
#19289=DIRECTION('center_axis',(1.,0.,0.));
#19290=DIRECTION('ref_axis',(0.,0.,-1.));
#19291=DIRECTION('',(0.,-1.,0.));
#19292=DIRECTION('',(0.,0.,-1.));
#19293=DIRECTION('',(0.,-1.,0.));
#19294=DIRECTION('center_axis',(0.,1.,0.));
#19295=DIRECTION('ref_axis',(0.,0.,1.));
#19296=DIRECTION('',(1.,0.,0.));
#19297=DIRECTION('',(1.,0.,0.));
#19298=DIRECTION('center_axis',(0.,0.,-1.));
#19299=DIRECTION('ref_axis',(-1.,0.,0.));
#19300=DIRECTION('center_axis',(0.,0.,-1.));
#19301=DIRECTION('ref_axis',(-1.,0.,0.));
#19302=DIRECTION('center_axis',(-1.,0.,0.));
#19303=DIRECTION('ref_axis',(0.,0.,1.));
#19304=DIRECTION('center_axis',(1.,0.,0.));
#19305=DIRECTION('ref_axis',(0.,0.,-1.));
#19306=DIRECTION('',(-1.,0.,0.));
#19307=DIRECTION('center_axis',(1.,0.,0.));
#19308=DIRECTION('ref_axis',(0.,0.,-1.));
#19309=DIRECTION('center_axis',(1.,0.,0.));
#19310=DIRECTION('ref_axis',(0.,0.,-1.));
#19311=DIRECTION('',(0.,-1.,0.));
#19312=DIRECTION('',(0.,-0.500011000363013,-0.866019052628739));
#19313=DIRECTION('',(0.,0.866029956157432,-0.499992114975783));
#19314=DIRECTION('',(0.,0.782106676792726,0.623144562775154));
#19315=DIRECTION('center_axis',(-1.,0.,0.));
#19316=DIRECTION('ref_axis',(0.,0.,-1.));
#19317=DIRECTION('',(0.,0.,1.));
#19318=DIRECTION('center_axis',(1.,0.,0.));
#19319=DIRECTION('ref_axis',(0.,0.,-1.));
#19320=DIRECTION('',(0.,-1.,0.));
#19321=DIRECTION('',(0.,0.,1.));
#19322=DIRECTION('center_axis',(-1.,0.,0.));
#19323=DIRECTION('ref_axis',(0.,0.,-1.));
#19324=DIRECTION('',(0.,0.782106676792726,0.623144562775154));
#19325=DIRECTION('',(0.,0.866029956157432,-0.499992114975783));
#19326=DIRECTION('',(0.,-0.500011000363013,-0.866019052628739));
#19327=DIRECTION('center_axis',(0.,0.,-1.));
#19328=DIRECTION('ref_axis',(-1.,0.,0.));
#19329=DIRECTION('',(-1.,0.,0.));
#19330=DIRECTION('',(-1.,0.,0.));
#19331=DIRECTION('center_axis',(0.,0.866019052628739,-0.500011000363013));
#19332=DIRECTION('ref_axis',(0.,0.500011000363013,0.866019052628739));
#19333=DIRECTION('',(-1.,0.,0.));
#19334=DIRECTION('center_axis',(0.,0.499992114975783,0.866029956157432));
#19335=DIRECTION('ref_axis',(0.,-0.866029956157432,0.499992114975783));
#19336=DIRECTION('',(-1.,0.,0.));
#19337=DIRECTION('center_axis',(0.,-0.623144562775154,0.782106676792726));
#19338=DIRECTION('ref_axis',(0.,-0.782106676792726,-0.623144562775154));
#19339=DIRECTION('',(-1.,0.,0.));
#19340=DIRECTION('center_axis',(-1.,0.,0.));
#19341=DIRECTION('ref_axis',(0.,0.,1.));
#19342=DIRECTION('',(-1.,0.,0.));
#19343=DIRECTION('center_axis',(0.,-1.,0.));
#19344=DIRECTION('ref_axis',(0.,0.,-1.));
#19345=DIRECTION('center_axis',(1.,0.,0.));
#19346=DIRECTION('ref_axis',(0.,0.,1.));
#19347=DIRECTION('center_axis',(1.,0.,0.));
#19348=DIRECTION('ref_axis',(0.,0.,-1.));
#19349=DIRECTION('',(1.,0.,0.));
#19350=DIRECTION('center_axis',(1.,0.,0.));
#19351=DIRECTION('ref_axis',(0.,0.,-1.));
#19352=DIRECTION('center_axis',(-1.,0.,0.));
#19353=DIRECTION('ref_axis',(0.,0.,-1.));
#19354=DIRECTION('',(0.,-1.,0.));
#19355=DIRECTION('',(0.,0.,1.));
#19356=DIRECTION('center_axis',(-1.,0.,0.));
#19357=DIRECTION('ref_axis',(0.,0.,-1.));
#19358=DIRECTION('',(0.,0.782106676792726,0.623144562775154));
#19359=DIRECTION('',(0.,0.866029956157432,-0.499992114975783));
#19360=DIRECTION('',(0.,-0.500011000363013,-0.866019052628739));
#19361=DIRECTION('center_axis',(-1.,0.,0.));
#19362=DIRECTION('ref_axis',(0.,0.,-1.));
#19363=DIRECTION('',(0.,-1.,0.));
#19364=DIRECTION('',(0.,-0.500011000363013,-0.866019052628739));
#19365=DIRECTION('',(0.,0.866029956157432,-0.499992114975783));
#19366=DIRECTION('',(0.,0.782106676792726,0.623144562775154));
#19367=DIRECTION('center_axis',(-1.,0.,0.));
#19368=DIRECTION('ref_axis',(0.,0.,-1.));
#19369=DIRECTION('',(0.,0.,1.));
#19370=DIRECTION('center_axis',(0.,0.,-1.));
#19371=DIRECTION('ref_axis',(1.,0.,0.));
#19372=DIRECTION('',(1.,0.,0.));
#19373=DIRECTION('',(1.,0.,0.));
#19374=DIRECTION('center_axis',(0.,0.866019052628739,-0.500011000363013));
#19375=DIRECTION('ref_axis',(0.,0.500011000363013,0.866019052628739));
#19376=DIRECTION('',(1.,0.,0.));
#19377=DIRECTION('center_axis',(0.,0.499992114975783,0.866029956157432));
#19378=DIRECTION('ref_axis',(0.,-0.866029956157432,0.499992114975783));
#19379=DIRECTION('',(1.,0.,0.));
#19380=DIRECTION('center_axis',(0.,-0.623144562775154,0.782106676792726));
#19381=DIRECTION('ref_axis',(0.,-0.782106676792726,-0.623144562775154));
#19382=DIRECTION('',(1.,0.,0.));
#19383=DIRECTION('center_axis',(1.,0.,0.));
#19384=DIRECTION('ref_axis',(0.,0.,1.));
#19385=DIRECTION('',(1.,0.,0.));
#19386=DIRECTION('center_axis',(0.,-1.,0.));
#19387=DIRECTION('ref_axis',(0.,0.,-1.));
#19388=DIRECTION('center_axis',(0.,0.499992114975783,0.866029956157432));
#19389=DIRECTION('ref_axis',(0.,-0.866029956157432,0.499992114975783));
#19390=DIRECTION('center_axis',(0.,-0.499992114975783,-0.866029956157432));
#19391=DIRECTION('ref_axis',(0.,0.866029956157432,-0.499992114975783));
#19392=DIRECTION('',(0.,0.499992114975783,0.866029956157432));
#19393=DIRECTION('center_axis',(0.,-0.499992114975783,-0.866029956157432));
#19394=DIRECTION('ref_axis',(0.,0.866029956157432,-0.499992114975783));
#19395=DIRECTION('center_axis',(0.,0.499992114975783,0.866029956157432));
#19396=DIRECTION('ref_axis',(0.,-0.866029956157432,0.499992114975783));
#19397=DIRECTION('center_axis',(0.,-0.499992114975783,-0.866029956157432));
#19398=DIRECTION('ref_axis',(0.,0.866029956157432,-0.499992114975783));
#19399=DIRECTION('',(0.,0.499992114975783,0.866029956157432));
#19400=DIRECTION('center_axis',(0.,-0.499992114975783,-0.866029956157432));
#19401=DIRECTION('ref_axis',(0.,0.866029956157432,-0.499992114975783));
#19402=DIRECTION('center_axis',(0.,0.499992114975783,0.866029956157432));
#19403=DIRECTION('ref_axis',(0.,-0.866029956157432,0.499992114975783));
#19404=DIRECTION('center_axis',(0.,-0.499992114975783,-0.866029956157432));
#19405=DIRECTION('ref_axis',(0.,0.866029956157432,-0.499992114975783));
#19406=DIRECTION('',(0.,0.499992114975783,0.866029956157432));
#19407=DIRECTION('center_axis',(0.,-0.499992114975783,-0.866029956157432));
#19408=DIRECTION('ref_axis',(0.,0.866029956157432,-0.499992114975783));
#19409=DIRECTION('center_axis',(0.,0.499992114975783,0.866029956157432));
#19410=DIRECTION('ref_axis',(0.,-0.866029956157432,0.499992114975783));
#19411=DIRECTION('center_axis',(0.,-0.499992114975783,-0.866029956157432));
#19412=DIRECTION('ref_axis',(0.,0.866029956157432,-0.499992114975783));
#19413=DIRECTION('',(0.,0.499992114975783,0.866029956157432));
#19414=DIRECTION('center_axis',(0.,-0.499992114975783,-0.866029956157432));
#19415=DIRECTION('ref_axis',(0.,0.866029956157432,-0.499992114975783));
#19416=DIRECTION('center_axis',(0.,0.499992114975783,0.866029956157432));
#19417=DIRECTION('ref_axis',(0.,-0.866029956157432,0.499992114975783));
#19418=DIRECTION('center_axis',(0.,-0.499992114975783,-0.866029956157432));
#19419=DIRECTION('ref_axis',(0.,0.866029956157432,-0.499992114975783));
#19420=DIRECTION('',(0.,0.499992114975783,0.866029956157432));
#19421=DIRECTION('center_axis',(0.,-0.499992114975783,-0.866029956157432));
#19422=DIRECTION('ref_axis',(0.,0.866029956157432,-0.499992114975783));
#19423=DIRECTION('center_axis',(0.,0.499992114975783,0.866029956157432));
#19424=DIRECTION('ref_axis',(0.,-0.866029956157432,0.499992114975783));
#19425=DIRECTION('',(0.,-0.866029956157432,0.499992114975783));
#19426=DIRECTION('',(-0.499722453489577,-0.750142665109869,0.433085963129978));
#19427=DIRECTION('',(0.,-0.866029956157433,0.499992114975782));
#19428=DIRECTION('',(-1.,0.,0.));
#19429=DIRECTION('',(0.,0.866029956157433,-0.499992114975782));
#19430=DIRECTION('',(-0.499722453489577,0.750142665109869,-0.433085963129978));
#19431=DIRECTION('',(0.,0.866029956157432,-0.499992114975783));
#19432=DIRECTION('',(1.,0.,0.));
#19433=DIRECTION('center_axis',(0.,0.499992114975783,0.866029956157432));
#19434=DIRECTION('ref_axis',(0.,-0.866029956157432,0.499992114975783));
#19435=DIRECTION('',(0.,-0.866029956157432,0.499992114975783));
#19436=DIRECTION('',(1.,0.,0.));
#19437=DIRECTION('',(0.,0.866029956157432,-0.499992114975783));
#19438=DIRECTION('',(-0.499722453489577,0.750142665109869,-0.433085963129978));
#19439=DIRECTION('',(0.,0.866029956157433,-0.499992114975782));
#19440=DIRECTION('',(-1.,0.,0.));
#19441=DIRECTION('',(0.,-0.866029956157433,0.499992114975782));
#19442=DIRECTION('',(-0.499722453489577,-0.750142665109869,0.433085963129978));
#19443=DIRECTION('center_axis',(-1.,0.,0.));
#19444=DIRECTION('ref_axis',(0.,0.,1.));
#19445=DIRECTION('',(0.,0.499992114975783,0.866029956157432));
#19446=DIRECTION('',(0.,0.499992114975783,0.866029956157432));
#19447=DIRECTION('center_axis',(-0.866185586048601,0.432774614486463,-0.249857286421141));
#19448=DIRECTION('ref_axis',(-0.446950695480888,-0.89455859271998,-3.10117349013882E-18));
#19449=DIRECTION('',(0.,0.499992114975783,0.866029956157432));
#19450=DIRECTION('center_axis',(-1.,0.,0.));
#19451=DIRECTION('ref_axis',(0.,0.,1.));
#19452=DIRECTION('',(0.,0.499992114975783,0.866029956157432));
#19453=DIRECTION('center_axis',(0.,0.866029956157432,-0.499992114975783));
#19454=DIRECTION('ref_axis',(0.,0.499992114975783,0.866029956157432));
#19455=DIRECTION('',(0.,0.499992114975783,0.866029956157432));
#19456=DIRECTION('center_axis',(1.,0.,0.));
#19457=DIRECTION('ref_axis',(0.,0.,-1.));
#19458=DIRECTION('',(0.,0.499992114975783,0.866029956157432));
#19459=DIRECTION('center_axis',(0.866185586048601,0.432774614486463,-0.249857286421141));
#19460=DIRECTION('ref_axis',(-0.446950695480888,0.89455859271998,3.10117349013882E-18));
#19461=DIRECTION('',(0.,0.499992114975783,0.866029956157432));
#19462=DIRECTION('center_axis',(1.,0.,0.));
#19463=DIRECTION('ref_axis',(0.,0.,-1.));
#19464=DIRECTION('',(0.,0.499992114975783,0.866029956157432));
#19465=DIRECTION('center_axis',(0.,-0.866029956157432,0.499992114975783));
#19466=DIRECTION('ref_axis',(0.,-0.499992114975783,-0.866029956157432));
#19467=DIRECTION('center_axis',(9.439207419131E-6,0.500006284256325,0.866021775485516));
#19468=DIRECTION('ref_axis',(5.27658532184428E-22,-0.866021775524096,0.5000062842786));
#19469=DIRECTION('',(0.499722453400429,0.750133220675019,-0.4331023214059));
#19470=DIRECTION('',(-0.866185586048601,0.432774614486463,-0.249857286421141));
#19471=DIRECTION('',(0.499722453400429,0.750133220675019,-0.4331023214059));
#19472=DIRECTION('',(-0.866185586048601,0.432774614486463,-0.249857286421141));
#19473=DIRECTION('center_axis',(-0.499722453400429,-0.750133220675019,0.4331023214059));
#19474=DIRECTION('ref_axis',(0.832237843570743,-0.55441876927889,-3.50686665358977E-17));
#19475=DIRECTION('',(9.43920741954911E-6,0.500006284256325,0.866021775485515));
#19476=DIRECTION('',(-0.866185586048601,0.432774614486463,-0.249857286421141));
#19477=DIRECTION('',(9.43920741954911E-6,0.500006284256325,0.866021775485515));
#19478=DIRECTION('center_axis',(-9.43920741930175E-6,-0.500006284256325,
-0.866021775485516));
#19479=DIRECTION('ref_axis',(-2.61520069381354E-22,0.866021775524096,-0.5000062842786));
#19480=DIRECTION('',(-0.499722453400429,-0.750133220675019,0.4331023214059));
#19481=DIRECTION('',(-0.866185586048601,0.432774614486463,-0.249857286421141));
#19482=DIRECTION('',(-0.499722453400429,-0.750133220675019,0.4331023214059));
#19483=DIRECTION('center_axis',(0.499722453400429,0.750133220675019,-0.4331023214059));
#19484=DIRECTION('ref_axis',(-0.832237843570743,0.55441876927889,2.11982739611214E-17));
#19485=DIRECTION('',(-9.43920741954911E-6,-0.500006284256325,-0.866021775485515));
#19486=DIRECTION('',(-9.43920741954911E-6,-0.500006284256325,-0.866021775485515));
#19487=DIRECTION('center_axis',(-0.866185586048601,0.432774614486463,-0.249857286421141));
#19488=DIRECTION('ref_axis',(-0.446950695480887,-0.89455859271998,-4.18661307789075E-19));
#19489=DIRECTION('center_axis',(-0.866185586048601,0.432774614486463,-0.249857286421141));
#19490=DIRECTION('ref_axis',(-0.446950695480887,-0.89455859271998,-4.18661307789075E-19));
#19491=DIRECTION('center_axis',(0.,0.500011000363013,0.866019052628739));
#19492=DIRECTION('ref_axis',(0.,-0.866019052628739,0.500011000363013));
#19493=DIRECTION('',(0.,0.866019052628739,-0.500011000363013));
#19494=DIRECTION('',(-1.,0.,0.));
#19495=DIRECTION('',(0.,0.866019052628739,-0.500011000363013));
#19496=DIRECTION('',(-1.,0.,0.));
#19497=DIRECTION('center_axis',(0.,-0.866019052628739,0.500011000363013));
#19498=DIRECTION('ref_axis',(0.,-0.500011000363013,-0.866019052628739));
#19499=DIRECTION('',(0.,0.500011000363013,0.866019052628739));
#19500=DIRECTION('',(-1.,0.,0.));
#19501=DIRECTION('',(0.,0.500011000363013,0.866019052628739));
#19502=DIRECTION('center_axis',(0.,-0.500011000363012,-0.86601905262874));
#19503=DIRECTION('ref_axis',(0.,0.86601905262874,-0.500011000363012));
#19504=DIRECTION('',(0.,-0.86601905262874,0.500011000363011));
#19505=DIRECTION('',(-1.,0.,0.));
#19506=DIRECTION('',(0.,-0.86601905262874,0.500011000363011));
#19507=DIRECTION('center_axis',(0.,0.866019052628739,-0.500011000363013));
#19508=DIRECTION('ref_axis',(0.,0.500011000363013,0.866019052628739));
#19509=DIRECTION('',(0.,-0.500011000363013,-0.866019052628739));
#19510=DIRECTION('',(0.,-0.500011000363013,-0.866019052628739));
#19511=DIRECTION('center_axis',(1.,0.,0.));
#19512=DIRECTION('ref_axis',(0.,0.,-1.));
#19513=DIRECTION('center_axis',(1.,0.,0.));
#19514=DIRECTION('ref_axis',(0.,0.,-1.));
#19515=DIRECTION('center_axis',(-0.866183663354203,0.432777500629603,-0.249858952785541));
#19516=DIRECTION('ref_axis',(-0.44695387464567,-0.894557004298341,2.04692415542437E-18));
#19517=DIRECTION('',(0.499725786055908,0.750131555564074,-0.433101360073861));
#19518=DIRECTION('',(-9.43920741916444E-6,-0.500006284256325,-0.866021775485515));
#19519=DIRECTION('',(0.499725786055908,0.750131555564074,-0.433101360073861));
#19520=DIRECTION('',(-9.43920741916444E-6,-0.500006284256325,-0.866021775485515));
#19521=DIRECTION('center_axis',(1.38189965515079E-17,-0.866021775524096,
0.5000062842786));
#19522=DIRECTION('ref_axis',(1.57777990579274E-34,-0.5000062842786,-0.866021775524096));
#19523=DIRECTION('',(-0.999999999955451,4.71966302817637E-6,8.17455916868661E-6));
#19524=DIRECTION('',(-9.43920741916444E-6,-0.500006284256325,-0.866021775485515));
#19525=DIRECTION('',(-0.999999999955451,4.71966302817637E-6,8.17455916868661E-6));
#19526=DIRECTION('center_axis',(0.866187508712929,0.432763552136484,-0.249869781470073));
#19527=DIRECTION('ref_axis',(-0.446940759058379,0.894563557212298,1.17495033585261E-17));
#19528=DIRECTION('',(0.499719120767447,-0.750139602771641,0.433095112755863));
#19529=DIRECTION('',(-9.43920741916444E-6,-0.500006284256325,-0.866021775485515));
#19530=DIRECTION('',(0.499719120767447,-0.750139602771641,0.433095112755863));
#19531=DIRECTION('center_axis',(0.999999999955451,-4.7196630281914E-6,-8.17455916868501E-6));
#19532=DIRECTION('ref_axis',(-8.17455916877606E-6,-2.91745525458034E-27,
-0.999999999966588));
#19533=DIRECTION('',(0.,-0.866021775524096,0.500006284278599));
#19534=DIRECTION('',(-9.43920741916444E-6,-0.500006284256325,-0.866021775485515));
#19535=DIRECTION('',(0.,-0.866021775524096,0.500006284278599));
#19536=DIRECTION('center_axis',(-1.3955513918745E-17,0.866021775524096,
-0.5000062842786));
#19537=DIRECTION('ref_axis',(4.04649682246767E-34,0.5000062842786,0.866021775524096));
#19538=DIRECTION('',(0.999999999955451,-4.71966302817428E-6,-8.17455916868326E-6));
#19539=DIRECTION('',(-9.43920741916444E-6,-0.500006284256325,-0.866021775485515));
#19540=DIRECTION('',(0.999999999955451,-4.71966302817428E-6,-8.17455916868326E-6));
#19541=DIRECTION('center_axis',(-0.999999999955451,4.7196630281914E-6,8.17455916868501E-6));
#19542=DIRECTION('ref_axis',(8.17455916877606E-6,2.91745525458034E-27,0.999999999966588));
#19543=DIRECTION('',(0.,0.866021775524096,-0.500006284278599));
#19544=DIRECTION('',(0.,0.866021775524097,-0.500006284278599));
#19545=DIRECTION('center_axis',(9.43920741915831E-6,0.500006284256325,0.866021775485515));
#19546=DIRECTION('ref_axis',(2.19424632593594E-22,-0.866021775524096,0.5000062842786));
#19547=DIRECTION('center_axis',(9.43920741915831E-6,0.500006284256325,0.866021775485515));
#19548=DIRECTION('ref_axis',(2.19424632593594E-22,-0.866021775524096,0.5000062842786));
#19549=DIRECTION('center_axis',(0.,0.866019052628739,-0.500011000363013));
#19550=DIRECTION('ref_axis',(0.,0.500011000363013,0.866019052628739));
#19551=DIRECTION('center_axis',(0.,-0.866019052628739,0.500011000363013));
#19552=DIRECTION('ref_axis',(0.,-0.500011000363013,-0.866019052628739));
#19553=DIRECTION('',(0.,0.866019052628739,-0.500011000363013));
#19554=DIRECTION('center_axis',(0.,-0.866019052628739,0.500011000363013));
#19555=DIRECTION('ref_axis',(0.,-0.500011000363013,-0.866019052628739));
#19556=DIRECTION('center_axis',(0.,0.866019052628739,-0.500011000363013));
#19557=DIRECTION('ref_axis',(0.,0.500011000363013,0.866019052628739));
#19558=DIRECTION('center_axis',(0.,-0.866019052628739,0.500011000363013));
#19559=DIRECTION('ref_axis',(0.,-0.500011000363013,-0.86601905262874));
#19560=DIRECTION('',(0.,0.866019052628739,-0.500011000363013));
#19561=DIRECTION('center_axis',(0.,-0.866019052628739,0.500011000363013));
#19562=DIRECTION('ref_axis',(0.,-0.500011000363013,-0.86601905262874));
#19563=DIRECTION('center_axis',(0.,0.866019052628739,-0.500011000363013));
#19564=DIRECTION('ref_axis',(0.,0.500011000363013,0.866019052628739));
#19565=DIRECTION('center_axis',(0.,-0.866019052628739,0.500011000363013));
#19566=DIRECTION('ref_axis',(0.,-0.500011000363013,-0.866019052628739));
#19567=DIRECTION('',(0.,0.866019052628739,-0.500011000363013));
#19568=DIRECTION('center_axis',(0.,-0.866019052628739,0.500011000363013));
#19569=DIRECTION('ref_axis',(0.,-0.500011000363013,-0.866019052628739));
#19570=DIRECTION('center_axis',(0.,-0.866019052628739,0.500011000363013));
#19571=DIRECTION('ref_axis',(0.,-0.500011000363013,-0.866019052628739));
#19572=DIRECTION('',(1.88173394004264E-16,-0.500011000363013,-0.866019052628739));
#19573=DIRECTION('',(1.,0.,0.));
#19574=DIRECTION('',(-1.88173394004264E-16,0.500011000363013,0.866019052628739));
#19575=DIRECTION('',(-1.,0.,0.));
#19576=DIRECTION('center_axis',(0.,-0.866019052628739,0.500011000363013));
#19577=DIRECTION('ref_axis',(0.,-0.500011000363013,-0.866019052628739));
#19578=DIRECTION('',(1.88173394004264E-16,-0.500011000363013,-0.866019052628739));
#19579=DIRECTION('',(-1.,0.,0.));
#19580=DIRECTION('',(-1.88173394004264E-16,0.500011000363013,0.866019052628739));
#19581=DIRECTION('',(1.,0.,0.));
#19582=DIRECTION('center_axis',(1.,9.40887669777753E-17,1.62961744405507E-16));
#19583=DIRECTION('ref_axis',(1.62961744405507E-16,0.,-1.));
#19584=DIRECTION('',(0.,0.866019052628739,-0.500011000363013));
#19585=DIRECTION('',(0.,0.866019052628739,-0.500011000363013));
#19586=DIRECTION('center_axis',(0.,0.500011000363013,0.866019052628739));
#19587=DIRECTION('ref_axis',(0.,-0.866019052628739,0.500011000363013));
#19588=DIRECTION('',(0.,0.866019052628739,-0.500011000363013));
#19589=DIRECTION('center_axis',(-1.,-9.40887669777753E-17,-1.62961744405507E-16));
#19590=DIRECTION('ref_axis',(-1.62961744405507E-16,0.,1.));
#19591=DIRECTION('',(0.,0.866019052628739,-0.500011000363013));
#19592=DIRECTION('center_axis',(0.,-0.500011000363013,-0.866019052628739));
#19593=DIRECTION('ref_axis',(0.,0.866019052628739,-0.500011000363013));
#19594=DIRECTION('center_axis',(5.44569658622596E-6,0.866021775511255,-0.500006284271186));
#19595=DIRECTION('ref_axis',(-0.999999999985172,4.71609182512488E-6,-2.72288251788859E-6));
#19596=DIRECTION('center_axis',(-5.44569658622596E-6,-0.866021775511255,
0.500006284271186));
#19597=DIRECTION('ref_axis',(0.999999999985172,-4.71609182512488E-6,2.72288251788859E-6));
#19598=DIRECTION('',(5.44569658622596E-6,0.866021775511255,-0.500006284271186));
#19599=DIRECTION('center_axis',(-5.44569658622596E-6,-0.866021775511255,
0.500006284271186));
#19600=DIRECTION('ref_axis',(0.999999999985172,-4.71609182512488E-6,2.72288251788859E-6));
#19601=DIRECTION('center_axis',(5.44569658622596E-6,0.866021775511255,-0.500006284271186));
#19602=DIRECTION('ref_axis',(-0.999999999985172,4.71609182512488E-6,-2.72288251788859E-6));
#19603=DIRECTION('center_axis',(-5.44569658622596E-6,-0.866021775511255,
0.500006284271186));
#19604=DIRECTION('ref_axis',(0.999999999985172,-4.71609182512488E-6,2.72288251788859E-6));
#19605=DIRECTION('',(5.44569658622596E-6,0.866021775511255,-0.500006284271186));
#19606=DIRECTION('center_axis',(-5.44569658622596E-6,-0.866021775511255,
0.500006284271186));
#19607=DIRECTION('ref_axis',(0.999999999985172,-4.71609182512488E-6,2.72288251788859E-6));
#19608=DIRECTION('center_axis',(5.44569658622596E-6,0.866021775511255,-0.500006284271186));
#19609=DIRECTION('ref_axis',(-0.999999999985172,4.71609182512488E-6,-2.72288251788859E-6));
#19610=DIRECTION('center_axis',(-5.44569658622596E-6,-0.866021775511255,
0.500006284271186));
#19611=DIRECTION('ref_axis',(0.999999999985172,-4.71609182512488E-6,2.72288251788859E-6));
#19612=DIRECTION('',(5.44569658622596E-6,0.866021775511255,-0.500006284271186));
#19613=DIRECTION('center_axis',(-5.44569658622596E-6,-0.866021775511255,
0.500006284271186));
#19614=DIRECTION('ref_axis',(0.999999999985172,-4.71609182512488E-6,2.72288251788859E-6));
#19615=DIRECTION('center_axis',(-5.44569658625102E-6,-0.866021775511255,
0.500006284271186));
#19616=DIRECTION('ref_axis',(0.999999999985172,-4.71609182484123E-6,2.72288251843E-6));
#19617=DIRECTION('',(0.999999999985172,-4.71609182473021E-6,2.72288251859654E-6));
#19618=DIRECTION('',(-3.49148133884313E-15,0.5000062842786,0.866021775524096));
#19619=DIRECTION('',(-0.999999999985172,4.71609182473021E-6,-2.72288251859654E-6));
#19620=DIRECTION('',(3.49148133884313E-15,-0.5000062842786,-0.866021775524096));
#19621=DIRECTION('center_axis',(-5.44569658625102E-6,-0.866021775511255,
0.500006284271186));
#19622=DIRECTION('ref_axis',(0.999999999985172,-4.71609182484123E-6,2.72288251843E-6));
#19623=DIRECTION('',(0.999999999985172,-4.71609182473021E-6,2.72288251859654E-6));
#19624=DIRECTION('',(3.49148133884313E-15,-0.5000062842786,-0.866021775524096));
#19625=DIRECTION('',(-0.999999999985172,4.71609182473021E-6,-2.72288251859654E-6));
#19626=DIRECTION('',(-3.49148133884313E-15,0.5000062842786,0.866021775524096));
#19627=DIRECTION('center_axis',(-3.71924713249427E-15,0.5000062842786,0.866021775524096));
#19628=DIRECTION('ref_axis',(0.866021775524096,0.433016330084161,-0.25000628431809));
#19629=DIRECTION('',(5.44569658622596E-6,0.866021775511255,-0.500006284271186));
#19630=DIRECTION('',(5.44569658622596E-6,0.866021775511255,-0.500006284271186));
#19631=DIRECTION('center_axis',(-0.999999999985172,4.71609182482138E-6,
-2.72288251841425E-6));
#19632=DIRECTION('ref_axis',(-5.44569658622595E-6,-0.866021775511255,0.500006284271186));
#19633=DIRECTION('',(5.44569658622596E-6,0.866021775511255,-0.500006284271186));
#19634=DIRECTION('center_axis',(3.71924713249427E-15,-0.5000062842786,-0.866021775524096));
#19635=DIRECTION('ref_axis',(-0.866021775524096,-0.433016330084161,0.25000628431809));
#19636=DIRECTION('',(5.44569658622596E-6,0.866021775511255,-0.500006284271186));
#19637=DIRECTION('center_axis',(0.999999999985172,-4.71609182482138E-6,
2.72288251841425E-6));
#19638=DIRECTION('ref_axis',(5.44569658622595E-6,0.866021775511255,-0.500006284271186));
#19639=DIRECTION('center_axis',(-2.79110278370762E-17,0.86602449839377,
-0.50000156817936));
#19640=DIRECTION('ref_axis',(6.68375889402081E-33,-0.50000156817936,-0.86602449839377));
#19641=DIRECTION('center_axis',(2.79110278370762E-17,-0.86602449839377,
0.50000156817936));
#19642=DIRECTION('ref_axis',(-6.68375889402081E-33,0.50000156817936,0.86602449839377));
#19643=DIRECTION('',(-2.79110278370762E-17,0.86602449839377,-0.50000156817936));
#19644=DIRECTION('center_axis',(2.79110278370762E-17,-0.86602449839377,
0.50000156817936));
#19645=DIRECTION('ref_axis',(-6.68375889402081E-33,0.50000156817936,0.86602449839377));
#19646=DIRECTION('center_axis',(-2.79110278370762E-17,0.86602449839377,
-0.50000156817936));
#19647=DIRECTION('ref_axis',(2.51726960247898E-32,-0.50000156817936,-0.86602449839377));
#19648=DIRECTION('center_axis',(2.79110278370762E-17,-0.86602449839377,
0.50000156817936));
#19649=DIRECTION('ref_axis',(-2.51726960247898E-32,0.50000156817936,0.86602449839377));
#19650=DIRECTION('',(-2.79110278370762E-17,0.86602449839377,-0.50000156817936));
#19651=DIRECTION('center_axis',(2.79110278370762E-17,-0.86602449839377,
0.50000156817936));
#19652=DIRECTION('ref_axis',(-2.51726960247898E-32,0.50000156817936,0.86602449839377));
#19653=DIRECTION('center_axis',(-2.79110278370762E-17,0.86602449839377,
-0.50000156817936));
#19654=DIRECTION('ref_axis',(-1.48866758124192E-32,-0.50000156817936,-0.86602449839377));
#19655=DIRECTION('center_axis',(2.79110278370762E-17,-0.86602449839377,
0.50000156817936));
#19656=DIRECTION('ref_axis',(1.48866758124192E-32,0.50000156817936,0.86602449839377));
#19657=DIRECTION('',(-2.79110278370762E-17,0.86602449839377,-0.50000156817936));
#19658=DIRECTION('center_axis',(2.79110278370762E-17,-0.86602449839377,
0.50000156817936));
#19659=DIRECTION('ref_axis',(1.48866758124192E-32,0.50000156817936,0.86602449839377));
#19660=DIRECTION('center_axis',(2.79110278370762E-17,-0.86602449839377,
0.50000156817936));
#19661=DIRECTION('ref_axis',(1.51994989013002E-22,0.50000156817936,0.86602449839377));
#19662=DIRECTION('',(-1.88173242009275E-16,0.50000156817936,0.86602449839377));
#19663=DIRECTION('',(-1.,-2.41715578845256E-17,1.395568931942E-17));
#19664=DIRECTION('',(1.88173242009275E-16,-0.50000156817936,-0.86602449839377));
#19665=DIRECTION('',(1.,2.41715578845256E-17,-1.395568931942E-17));
#19666=DIRECTION('center_axis',(2.79110278370762E-17,-0.86602449839377,
0.50000156817936));
#19667=DIRECTION('ref_axis',(1.51994989013002E-22,0.50000156817936,0.86602449839377));
#19668=DIRECTION('',(-1.88173242009275E-16,0.50000156817936,0.86602449839377));
#19669=DIRECTION('',(1.,2.41715578845256E-17,-1.395568931942E-17));
#19670=DIRECTION('',(1.88173242009275E-16,-0.50000156817936,-0.86602449839377));
#19671=DIRECTION('',(-1.,-2.41715578845256E-17,1.395568931942E-17));
#19672=DIRECTION('center_axis',(-1.,-1.1825854997629E-16,-1.49007079834176E-16));
#19673=DIRECTION('ref_axis',(-1.76917433724927E-16,0.866032660168318,0.499987431363815));
#19674=DIRECTION('',(-2.79110278370762E-17,0.86602449839377,-0.50000156817936));
#19675=DIRECTION('',(-2.79110278370762E-17,0.86602449839377,-0.50000156817936));
#19676=DIRECTION('center_axis',(-1.51994989007369E-22,-0.50000156817936,
-0.86602449839377));
#19677=DIRECTION('ref_axis',(2.79110278370762E-17,-0.86602449839377,0.50000156817936));
#19678=DIRECTION('',(-2.79110278370762E-17,0.86602449839377,-0.50000156817936));
#19679=DIRECTION('center_axis',(1.,1.1825854997629E-16,1.49007079834176E-16));
#19680=DIRECTION('ref_axis',(1.76917433724927E-16,-0.866032660168318,-0.499987431363815));
#19681=DIRECTION('',(-2.79110278370762E-17,0.86602449839377,-0.50000156817936));
#19682=DIRECTION('center_axis',(1.51994989007369E-22,0.50000156817936,0.86602449839377));
#19683=DIRECTION('ref_axis',(-2.79110278370762E-17,0.86602449839377,-0.50000156817936));
#19684=DIRECTION('center_axis',(-5.44569658622596E-6,0.866021775511255,
-0.500006284271186));
#19685=DIRECTION('ref_axis',(0.999999999985172,4.71609183046649E-6,-2.72288250863681E-6));
#19686=DIRECTION('center_axis',(5.44569658622596E-6,-0.866021775511255,
0.500006284271186));
#19687=DIRECTION('ref_axis',(-0.999999999985172,-4.71609183046649E-6,2.72288250863681E-6));
#19688=DIRECTION('',(-5.44569658622596E-6,0.866021775511255,-0.500006284271186));
#19689=DIRECTION('center_axis',(5.44569658622596E-6,-0.866021775511255,
0.500006284271186));
#19690=DIRECTION('ref_axis',(-0.999999999985172,-4.71609183046649E-6,2.72288250863681E-6));
#19691=DIRECTION('center_axis',(-5.44569658622596E-6,0.866021775511255,
-0.500006284271186));
#19692=DIRECTION('ref_axis',(0.999999999985172,4.71609183046649E-6,-2.72288250863681E-6));
#19693=DIRECTION('center_axis',(5.44569658622596E-6,-0.866021775511255,
0.500006284271186));
#19694=DIRECTION('ref_axis',(-0.999999999985172,-4.71609183046649E-6,2.72288250863681E-6));
#19695=DIRECTION('',(-5.44569658622596E-6,0.866021775511255,-0.500006284271186));
#19696=DIRECTION('center_axis',(5.44569658622596E-6,-0.866021775511255,
0.500006284271186));
#19697=DIRECTION('ref_axis',(-0.999999999985172,-4.71609183046649E-6,2.72288250863681E-6));
#19698=DIRECTION('center_axis',(-5.44569658622596E-6,0.866021775511255,
-0.500006284271186));
#19699=DIRECTION('ref_axis',(0.999999999985172,4.71609183046649E-6,-2.72288250863681E-6));
#19700=DIRECTION('center_axis',(5.44569658622596E-6,-0.866021775511255,
0.500006284271186));
#19701=DIRECTION('ref_axis',(-0.999999999985172,-4.71609183046649E-6,2.72288250863681E-6));
#19702=DIRECTION('',(-5.44569658622596E-6,0.866021775511255,-0.500006284271186));
#19703=DIRECTION('center_axis',(5.44569658622596E-6,-0.866021775511255,
0.500006284271186));
#19704=DIRECTION('ref_axis',(-0.999999999985172,-4.71609183046649E-6,2.72288250863681E-6));
#19705=DIRECTION('center_axis',(5.44569658619558E-6,-0.866021775511255,
0.500006284271186));
#19706=DIRECTION('ref_axis',(-0.999999999985172,-4.71609183178012E-6,2.72288250630082E-6));
#19707=DIRECTION('',(-0.999999999985172,-4.71609183189114E-6,2.72288250613428E-6));
#19708=DIRECTION('',(1.04744440165294E-14,-0.5000062842786,-0.866021775524096));
#19709=DIRECTION('',(0.999999999985172,4.71609183189114E-6,-2.72288250613428E-6));
#19710=DIRECTION('',(-1.04744440165294E-14,0.5000062842786,0.866021775524096));
#19711=DIRECTION('center_axis',(5.44569658619558E-6,-0.866021775511255,
0.500006284271186));
#19712=DIRECTION('ref_axis',(-0.999999999985172,-4.71609183178012E-6,2.72288250630082E-6));
#19713=DIRECTION('',(-0.999999999985172,-4.71609183189114E-6,2.72288250613428E-6));
#19714=DIRECTION('',(-1.04744440165294E-14,0.5000062842786,0.866021775524096));
#19715=DIRECTION('',(0.999999999985172,4.71609183189114E-6,-2.72288250613428E-6));
#19716=DIRECTION('',(1.04744440165294E-14,-0.5000062842786,-0.866021775524096));
#19717=DIRECTION('center_axis',(1.06303854607859E-14,-0.5000062842786,-0.866021775524096));
#19718=DIRECTION('ref_axis',(-0.866021775524096,0.433016330084155,-0.2500062843181));
#19719=DIRECTION('',(-5.44569658622596E-6,0.866021775511255,-0.500006284271186));
#19720=DIRECTION('',(-5.44569658622596E-6,0.866021775511255,-0.500006284271186));
#19721=DIRECTION('center_axis',(0.999999999985172,4.71609183179441E-6,-2.72288250633682E-6));
#19722=DIRECTION('ref_axis',(5.44569658622596E-6,-0.866021775511255,0.500006284271186));
#19723=DIRECTION('',(-5.44569658622596E-6,0.866021775511255,-0.500006284271186));
#19724=DIRECTION('center_axis',(-1.06303854607859E-14,0.5000062842786,0.866021775524096));
#19725=DIRECTION('ref_axis',(0.866021775524096,-0.433016330084155,0.2500062843181));
#19726=DIRECTION('',(-5.44569658622596E-6,0.866021775511255,-0.500006284271186));
#19727=DIRECTION('center_axis',(-0.999999999985172,-4.71609183179441E-6,
2.72288250633682E-6));
#19728=DIRECTION('ref_axis',(-5.44569658622596E-6,0.866021775511255,-0.500006284271186));
#19729=DIRECTION('center_axis',(-9.439207419131E-6,0.500006284256325,0.866021775485516));
#19730=DIRECTION('ref_axis',(-5.27658532184428E-22,-0.866021775524096,0.5000062842786));
#19731=DIRECTION('',(-0.499722453400429,0.750133220675019,-0.4331023214059));
#19732=DIRECTION('',(0.866185586048601,0.432774614486463,-0.249857286421141));
#19733=DIRECTION('',(-0.499722453400429,0.750133220675019,-0.4331023214059));
#19734=DIRECTION('',(0.866185586048601,0.432774614486463,-0.249857286421141));
#19735=DIRECTION('center_axis',(0.499722453400429,-0.750133220675019,0.4331023214059));
#19736=DIRECTION('ref_axis',(-0.832237843570743,-0.55441876927889,-3.50686665358977E-17));
#19737=DIRECTION('',(-9.43920741954911E-6,0.500006284256325,0.866021775485515));
#19738=DIRECTION('',(-9.43920741954911E-6,0.500006284256325,0.866021775485515));
#19739=DIRECTION('',(0.866185586048601,0.432774614486463,-0.249857286421141));
#19740=DIRECTION('center_axis',(9.43920741930175E-6,-0.500006284256325,
-0.866021775485516));
#19741=DIRECTION('ref_axis',(2.61520069381354E-22,0.866021775524096,-0.5000062842786));
#19742=DIRECTION('',(0.499722453400429,-0.750133220675019,0.4331023214059));
#19743=DIRECTION('',(0.499722453400429,-0.750133220675019,0.4331023214059));
#19744=DIRECTION('',(0.866185586048601,0.432774614486463,-0.249857286421141));
#19745=DIRECTION('center_axis',(-0.499722453400429,0.750133220675019,-0.4331023214059));
#19746=DIRECTION('ref_axis',(0.832237843570743,0.55441876927889,2.11982739611214E-17));
#19747=DIRECTION('',(9.43920741954911E-6,-0.500006284256325,-0.866021775485515));
#19748=DIRECTION('',(9.43920741954911E-6,-0.500006284256325,-0.866021775485515));
#19749=DIRECTION('center_axis',(0.866185586048601,0.432774614486463,-0.249857286421141));
#19750=DIRECTION('ref_axis',(0.446950695480887,-0.89455859271998,-4.18661307789075E-19));
#19751=DIRECTION('center_axis',(0.866185586048601,0.432774614486463,-0.249857286421141));
#19752=DIRECTION('ref_axis',(0.446950695480887,-0.89455859271998,-4.18661307789075E-19));
#19753=DIRECTION('center_axis',(0.,0.500011000363013,0.866019052628739));
#19754=DIRECTION('ref_axis',(0.,-0.866019052628739,0.500011000363013));
#19755=DIRECTION('',(0.,0.866019052628739,-0.500011000363013));
#19756=DIRECTION('',(1.,0.,0.));
#19757=DIRECTION('',(0.,0.866019052628739,-0.500011000363013));
#19758=DIRECTION('',(1.,0.,0.));
#19759=DIRECTION('center_axis',(0.,-0.866019052628739,0.500011000363013));
#19760=DIRECTION('ref_axis',(0.,-0.500011000363013,-0.866019052628739));
#19761=DIRECTION('',(0.,0.500011000363013,0.866019052628739));
#19762=DIRECTION('',(0.,0.500011000363013,0.866019052628739));
#19763=DIRECTION('',(1.,0.,0.));
#19764=DIRECTION('center_axis',(0.,-0.500011000363012,-0.86601905262874));
#19765=DIRECTION('ref_axis',(0.,0.86601905262874,-0.500011000363012));
#19766=DIRECTION('',(0.,-0.86601905262874,0.500011000363011));
#19767=DIRECTION('',(0.,-0.86601905262874,0.500011000363011));
#19768=DIRECTION('',(1.,0.,0.));
#19769=DIRECTION('center_axis',(0.,0.866019052628739,-0.500011000363013));
#19770=DIRECTION('ref_axis',(0.,0.500011000363013,0.866019052628739));
#19771=DIRECTION('',(0.,-0.500011000363013,-0.866019052628739));
#19772=DIRECTION('',(0.,-0.500011000363013,-0.866019052628739));
#19773=DIRECTION('center_axis',(-1.,0.,0.));
#19774=DIRECTION('ref_axis',(0.,0.,-1.));
#19775=DIRECTION('center_axis',(-1.,0.,0.));
#19776=DIRECTION('ref_axis',(0.,0.,-1.));
#19777=DIRECTION('center_axis',(1.,0.,0.));
#19778=DIRECTION('ref_axis',(0.,0.,-1.));
#19779=DIRECTION('',(0.,0.,1.));
#19780=DIRECTION('',(0.,-1.,0.));
#19781=DIRECTION('',(0.,0.,1.));
#19782=DIRECTION('',(0.,-1.,0.));
#19783=DIRECTION('center_axis',(0.,0.,-1.));
#19784=DIRECTION('ref_axis',(-1.,0.,0.));
#19785=DIRECTION('',(1.,0.,0.));
#19786=DIRECTION('',(0.,-1.,0.));
#19787=DIRECTION('',(1.,0.,0.));
#19788=DIRECTION('center_axis',(-1.,0.,0.));
#19789=DIRECTION('ref_axis',(0.,0.,1.));
#19790=DIRECTION('',(0.,0.,-1.));
#19791=DIRECTION('',(0.,-1.,0.));
#19792=DIRECTION('',(0.,0.,-1.));
#19793=DIRECTION('center_axis',(0.,0.,1.));
#19794=DIRECTION('ref_axis',(1.,0.,0.));
#19795=DIRECTION('',(-1.,0.,0.));
#19796=DIRECTION('',(-1.,0.,0.));
#19797=DIRECTION('center_axis',(0.,-1.,0.));
#19798=DIRECTION('ref_axis',(0.,0.,-1.));
#19799=DIRECTION('center_axis',(0.,-1.,0.));
#19800=DIRECTION('ref_axis',(0.,0.,-1.));
#19801=DIRECTION('center_axis',(-1.,0.,0.));
#19802=DIRECTION('ref_axis',(0.,0.,1.));
#19803=DIRECTION('',(0.,0.,1.));
#19804=DIRECTION('',(0.,1.,0.));
#19805=DIRECTION('',(0.,0.,1.));
#19806=DIRECTION('',(0.,1.,0.));
#19807=DIRECTION('center_axis',(-1.09275353725347E-14,0.,-1.));
#19808=DIRECTION('ref_axis',(-1.,0.,1.09275353725347E-14));
#19809=DIRECTION('',(-1.,0.,1.09275353725347E-14));
#19810=DIRECTION('',(0.,1.,0.));
#19811=DIRECTION('',(-1.,0.,1.09275353725347E-14));
#19812=DIRECTION('center_axis',(1.,0.,-1.04157383973362E-14));
#19813=DIRECTION('ref_axis',(-1.04157383973362E-14,0.,-1.));
#19814=DIRECTION('',(-1.04157383973362E-14,0.,-1.));
#19815=DIRECTION('',(0.,1.,0.));
#19816=DIRECTION('',(-1.04157383973362E-14,0.,-1.));
#19817=DIRECTION('center_axis',(0.,0.,1.));
#19818=DIRECTION('ref_axis',(1.,0.,0.));
#19819=DIRECTION('',(1.,0.,0.));
#19820=DIRECTION('',(1.,0.,0.));
#19821=DIRECTION('center_axis',(0.,1.,0.));
#19822=DIRECTION('ref_axis',(0.,0.,1.));
#19823=DIRECTION('center_axis',(0.,1.,0.));
#19824=DIRECTION('ref_axis',(0.,0.,1.));
#19825=DIRECTION('center_axis',(1.,0.,0.));
#19826=DIRECTION('ref_axis',(0.,0.,1.));
#19827=DIRECTION('',(0.,0.,1.));
#19828=DIRECTION('',(0.,1.,0.));
#19829=DIRECTION('',(0.,0.,1.));
#19830=DIRECTION('',(0.,1.,0.));
#19831=DIRECTION('center_axis',(1.09275353725347E-14,0.,-1.));
#19832=DIRECTION('ref_axis',(1.,0.,1.09275353725347E-14));
#19833=DIRECTION('',(1.,0.,1.09275353725347E-14));
#19834=DIRECTION('',(1.,0.,1.09275353725347E-14));
#19835=DIRECTION('',(0.,1.,0.));
#19836=DIRECTION('center_axis',(-1.,0.,-1.04157383973362E-14));
#19837=DIRECTION('ref_axis',(1.04157383973362E-14,0.,-1.));
#19838=DIRECTION('',(1.04157383973362E-14,0.,-1.));
#19839=DIRECTION('',(1.04157383973362E-14,0.,-1.));
#19840=DIRECTION('',(0.,1.,0.));
#19841=DIRECTION('center_axis',(0.,0.,1.));
#19842=DIRECTION('ref_axis',(-1.,0.,0.));
#19843=DIRECTION('',(-1.,0.,0.));
#19844=DIRECTION('',(-1.,0.,0.));
#19845=DIRECTION('center_axis',(0.,1.,0.));
#19846=DIRECTION('ref_axis',(0.,0.,1.));
#19847=DIRECTION('center_axis',(0.,1.,0.));
#19848=DIRECTION('ref_axis',(0.,0.,1.));
#19849=DIRECTION('center_axis',(0.,1.,0.));
#19850=DIRECTION('ref_axis',(0.,0.,1.));
#19851=DIRECTION('center_axis',(0.,-1.,0.));
#19852=DIRECTION('ref_axis',(0.,0.,-1.));
#19853=DIRECTION('',(0.,1.,0.));
#19854=DIRECTION('center_axis',(0.,-1.,0.));
#19855=DIRECTION('ref_axis',(0.,0.,-1.));
#19856=DIRECTION('center_axis',(0.,1.,0.));
#19857=DIRECTION('ref_axis',(0.,0.,1.));
#19858=DIRECTION('center_axis',(0.,-1.,0.));
#19859=DIRECTION('ref_axis',(0.,0.,-1.));
#19860=DIRECTION('',(0.,1.,0.));
#19861=DIRECTION('center_axis',(0.,-1.,0.));
#19862=DIRECTION('ref_axis',(0.,0.,-1.));
#19863=DIRECTION('center_axis',(0.,1.,0.));
#19864=DIRECTION('ref_axis',(0.,0.,1.));
#19865=DIRECTION('center_axis',(0.,-1.,0.));
#19866=DIRECTION('ref_axis',(0.,0.,-1.));
#19867=DIRECTION('',(0.,1.,0.));
#19868=DIRECTION('center_axis',(0.,-1.,0.));
#19869=DIRECTION('ref_axis',(0.,0.,-1.));
#19870=DIRECTION('center_axis',(0.,1.,0.));
#19871=DIRECTION('ref_axis',(0.,0.,1.));
#19872=DIRECTION('center_axis',(0.,-1.,0.));
#19873=DIRECTION('ref_axis',(0.,0.,-1.));
#19874=DIRECTION('',(0.,1.,0.));
#19875=DIRECTION('center_axis',(0.,-1.,0.));
#19876=DIRECTION('ref_axis',(0.,0.,-1.));
#19877=DIRECTION('center_axis',(0.,1.,0.));
#19878=DIRECTION('ref_axis',(0.,0.,1.));
#19879=DIRECTION('',(2.36721327212187E-16,0.,-1.));
#19880=DIRECTION('',(1.,0.,-3.03339624214524E-16));
#19881=DIRECTION('',(-2.36721327212187E-16,0.,1.));
#19882=DIRECTION('',(-1.,0.,-1.13752359080446E-16));
#19883=DIRECTION('center_axis',(0.,1.,0.));
#19884=DIRECTION('ref_axis',(0.,0.,1.));
#19885=DIRECTION('',(2.36721327212187E-16,0.,-1.));
#19886=DIRECTION('',(-1.,0.,-1.13752359080446E-16));
#19887=DIRECTION('',(-2.36721327212187E-16,0.,1.));
#19888=DIRECTION('',(1.,0.,-3.03339624214524E-16));
#19889=DIRECTION('center_axis',(1.,0.,2.36721327212187E-16));
#19890=DIRECTION('ref_axis',(2.36721327212187E-16,0.,-1.));
#19891=DIRECTION('',(0.,1.,0.));
#19892=DIRECTION('',(0.,1.,0.));
#19893=DIRECTION('center_axis',(3.03339624214524E-16,0.,1.));
#19894=DIRECTION('ref_axis',(1.,0.,-3.03339624214524E-16));
#19895=DIRECTION('',(0.,1.,0.));
#19896=DIRECTION('center_axis',(-1.,0.,-2.36721327212187E-16));
#19897=DIRECTION('ref_axis',(-2.36721327212187E-16,0.,1.));
#19898=DIRECTION('',(0.,1.,0.));
#19899=DIRECTION('center_axis',(1.13752359080446E-16,0.,-1.));
#19900=DIRECTION('ref_axis',(-1.,0.,-1.13752359080446E-16));
#19901=DIRECTION('center_axis',(0.,-1.,0.));
#19902=DIRECTION('ref_axis',(0.,0.,-1.));
#19903=DIRECTION('center_axis',(0.,-1.,0.));
#19904=DIRECTION('ref_axis',(0.,0.,-1.));
#19905=DIRECTION('',(0.,-1.,0.));
#19906=DIRECTION('center_axis',(0.,-1.,0.));
#19907=DIRECTION('ref_axis',(0.,0.,-1.));
#19908=DIRECTION('center_axis',(0.,-1.,0.));
#19909=DIRECTION('ref_axis',(0.,0.,-1.));
#19910=DIRECTION('center_axis',(0.,-1.,0.));
#19911=DIRECTION('ref_axis',(0.,0.,-1.));
#19912=DIRECTION('',(0.,-1.,0.));
#19913=DIRECTION('center_axis',(0.,-1.,0.));
#19914=DIRECTION('ref_axis',(0.,0.,-1.));
#19915=DIRECTION('center_axis',(0.,-1.,0.));
#19916=DIRECTION('ref_axis',(0.,0.,-1.));
#19917=DIRECTION('center_axis',(0.,-1.,0.));
#19918=DIRECTION('ref_axis',(0.,0.,-1.));
#19919=DIRECTION('',(0.,-1.,0.));
#19920=DIRECTION('center_axis',(0.,-1.,0.));
#19921=DIRECTION('ref_axis',(0.,0.,-1.));
#19922=DIRECTION('center_axis',(0.,-1.,0.));
#19923=DIRECTION('ref_axis',(0.,0.,-1.));
#19924=DIRECTION('center_axis',(0.,-1.,0.));
#19925=DIRECTION('ref_axis',(0.,0.,-1.));
#19926=DIRECTION('',(0.,-1.,0.));
#19927=DIRECTION('center_axis',(0.,-1.,0.));
#19928=DIRECTION('ref_axis',(0.,0.,-1.));
#19929=DIRECTION('center_axis',(0.,-1.,0.));
#19930=DIRECTION('ref_axis',(0.,0.,-1.));
#19931=DIRECTION('center_axis',(0.,-1.,0.));
#19932=DIRECTION('ref_axis',(0.,0.,-1.));
#19933=DIRECTION('',(0.,-1.,0.));
#19934=DIRECTION('center_axis',(0.,-1.,0.));
#19935=DIRECTION('ref_axis',(0.,0.,-1.));
#19936=DIRECTION('center_axis',(0.,-1.,0.));
#19937=DIRECTION('ref_axis',(0.,0.,-1.));
#19938=DIRECTION('center_axis',(0.,-1.,0.));
#19939=DIRECTION('ref_axis',(0.,0.,-1.));
#19940=DIRECTION('',(0.,-1.,0.));
#19941=DIRECTION('center_axis',(0.,-1.,0.));
#19942=DIRECTION('ref_axis',(0.,0.,-1.));
#19943=DIRECTION('center_axis',(1.,0.,0.));
#19944=DIRECTION('ref_axis',(0.,0.,-1.));
#19945=DIRECTION('',(0.,0.,1.));
#19946=DIRECTION('',(0.,-1.,0.));
#19947=DIRECTION('',(0.,0.,1.));
#19948=DIRECTION('',(0.,-1.,0.));
#19949=DIRECTION('center_axis',(1.22307178094722E-16,0.,-1.));
#19950=DIRECTION('ref_axis',(-1.,0.,-1.22307178094722E-16));
#19951=DIRECTION('',(1.,0.,1.22307178094722E-16));
#19952=DIRECTION('',(0.,-1.,0.));
#19953=DIRECTION('',(1.,0.,1.22307178094722E-16));
#19954=DIRECTION('center_axis',(-1.,0.,0.));
#19955=DIRECTION('ref_axis',(0.,0.,1.));
#19956=DIRECTION('',(0.,0.,-1.));
#19957=DIRECTION('',(0.,-1.,0.));
#19958=DIRECTION('',(0.,0.,-1.));
#19959=DIRECTION('center_axis',(-9.31864214055025E-17,0.,1.));
#19960=DIRECTION('ref_axis',(1.,0.,9.31864214055025E-17));
#19961=DIRECTION('',(-1.,0.,-9.31864214055025E-17));
#19962=DIRECTION('',(-1.,0.,-9.31864214055025E-17));
#19963=DIRECTION('center_axis',(0.,-1.,0.));
#19964=DIRECTION('ref_axis',(0.,0.,-1.));
#19965=DIRECTION('center_axis',(0.,-1.,0.));
#19966=DIRECTION('ref_axis',(0.,0.,-1.));
#19967=DIRECTION('center_axis',(-0.400352069216121,-0.916361402872453,0.));
#19968=DIRECTION('ref_axis',(0.916361402872453,-0.400352069216121,0.));
#19969=DIRECTION('',(0.916361402872453,-0.400352069216121,0.));
#19970=DIRECTION('',(0.,0.,1.));
#19971=DIRECTION('',(0.916361402872453,-0.400352069216121,0.));
#19972=DIRECTION('',(0.,0.,1.));
#19973=DIRECTION('center_axis',(-1.,0.,0.));
#19974=DIRECTION('ref_axis',(0.,0.,1.));
#19975=DIRECTION('',(0.,-1.,0.));
#19976=DIRECTION('',(0.,0.,1.));
#19977=DIRECTION('',(0.,-1.,0.));
#19978=DIRECTION('center_axis',(1.92747052886312E-16,1.,0.));
#19979=DIRECTION('ref_axis',(-1.,1.92747052886312E-16,0.));
#19980=DIRECTION('',(-1.,1.92747052886312E-16,0.));
#19981=DIRECTION('',(0.,0.,1.));
#19982=DIRECTION('',(-1.,1.92747052886312E-16,0.));
#19983=DIRECTION('center_axis',(0.707106781186551,0.707106781186544,0.));
#19984=DIRECTION('ref_axis',(-0.707106781186544,0.707106781186551,0.));
#19985=DIRECTION('',(-0.707106781186544,0.707106781186551,0.));
#19986=DIRECTION('',(0.,0.,1.));
#19987=DIRECTION('',(-0.707106781186544,0.707106781186551,0.));
#19988=DIRECTION('center_axis',(1.,0.,0.));
#19989=DIRECTION('ref_axis',(0.,0.,-1.));
#19990=DIRECTION('',(0.,1.,0.));
#19991=DIRECTION('',(0.,0.,1.));
#19992=DIRECTION('',(0.,1.,0.));
#19993=DIRECTION('center_axis',(0.707106781186546,-0.707106781186549,0.));
#19994=DIRECTION('ref_axis',(0.707106781186549,0.707106781186546,0.));
#19995=DIRECTION('',(0.707106781186549,0.707106781186546,0.));
#19996=DIRECTION('',(0.,0.,1.));
#19997=DIRECTION('',(0.707106781186549,0.707106781186546,0.));
#19998=DIRECTION('center_axis',(1.35393051783556E-15,-1.,0.));
#19999=DIRECTION('ref_axis',(1.,1.35393051783556E-15,0.));
#20000=DIRECTION('',(1.,1.35393051783556E-15,0.));
#20001=DIRECTION('',(1.,1.35393051783556E-15,0.));
#20002=DIRECTION('center_axis',(0.,0.,1.));
#20003=DIRECTION('ref_axis',(1.,0.,0.));
#20004=DIRECTION('center_axis',(0.,0.,1.));
#20005=DIRECTION('ref_axis',(1.,0.,0.));
#20006=DIRECTION('center_axis',(-0.400352069216121,-0.916361402872453,0.));
#20007=DIRECTION('ref_axis',(0.916361402872453,-0.400352069216121,0.));
#20008=DIRECTION('',(0.916361402872453,-0.400352069216121,0.));
#20009=DIRECTION('',(0.,0.,1.));
#20010=DIRECTION('',(0.916361402872453,-0.400352069216121,0.));
#20011=DIRECTION('',(0.,0.,1.));
#20012=DIRECTION('center_axis',(-1.,0.,0.));
#20013=DIRECTION('ref_axis',(0.,0.,1.));
#20014=DIRECTION('',(0.,-1.,0.));
#20015=DIRECTION('',(0.,0.,1.));
#20016=DIRECTION('',(0.,-1.,0.));
#20017=DIRECTION('center_axis',(1.92747052886312E-16,1.,0.));
#20018=DIRECTION('ref_axis',(-1.,1.92747052886312E-16,0.));
#20019=DIRECTION('',(-1.,1.92747052886312E-16,0.));
#20020=DIRECTION('',(0.,0.,1.));
#20021=DIRECTION('',(-1.,1.92747052886312E-16,0.));
#20022=DIRECTION('center_axis',(0.707106781186551,0.707106781186544,0.));
#20023=DIRECTION('ref_axis',(-0.707106781186544,0.707106781186551,0.));
#20024=DIRECTION('',(-0.707106781186544,0.707106781186551,0.));
#20025=DIRECTION('',(0.,0.,1.));
#20026=DIRECTION('',(-0.707106781186544,0.707106781186551,0.));
#20027=DIRECTION('center_axis',(1.,0.,0.));
#20028=DIRECTION('ref_axis',(0.,0.,-1.));
#20029=DIRECTION('',(0.,1.,0.));
#20030=DIRECTION('',(0.,0.,1.));
#20031=DIRECTION('',(0.,1.,0.));
#20032=DIRECTION('center_axis',(0.707106781186546,-0.707106781186549,0.));
#20033=DIRECTION('ref_axis',(0.707106781186549,0.707106781186546,0.));
#20034=DIRECTION('',(0.707106781186549,0.707106781186546,0.));
#20035=DIRECTION('',(0.,0.,1.));
#20036=DIRECTION('',(0.707106781186549,0.707106781186546,0.));
#20037=DIRECTION('center_axis',(1.35393051783556E-15,-1.,0.));
#20038=DIRECTION('ref_axis',(1.,1.35393051783556E-15,0.));
#20039=DIRECTION('',(1.,1.35393051783556E-15,0.));
#20040=DIRECTION('',(1.,1.35393051783556E-15,0.));
#20041=DIRECTION('center_axis',(0.,0.,1.));
#20042=DIRECTION('ref_axis',(1.,0.,0.));
#20043=DIRECTION('center_axis',(0.,0.,1.));
#20044=DIRECTION('ref_axis',(1.,0.,0.));
#20045=DIRECTION('center_axis',(-0.400352069216121,-0.916361402872453,0.));
#20046=DIRECTION('ref_axis',(0.916361402872453,-0.400352069216121,0.));
#20047=DIRECTION('',(0.916361402872453,-0.400352069216121,0.));
#20048=DIRECTION('',(0.,0.,1.));
#20049=DIRECTION('',(0.916361402872453,-0.400352069216121,0.));
#20050=DIRECTION('',(0.,0.,1.));
#20051=DIRECTION('center_axis',(-1.,0.,0.));
#20052=DIRECTION('ref_axis',(0.,0.,1.));
#20053=DIRECTION('',(0.,-1.,0.));
#20054=DIRECTION('',(0.,0.,1.));
#20055=DIRECTION('',(0.,-1.,0.));
#20056=DIRECTION('center_axis',(1.92747052886312E-16,1.,0.));
#20057=DIRECTION('ref_axis',(-1.,1.92747052886312E-16,0.));
#20058=DIRECTION('',(-1.,1.92747052886312E-16,0.));
#20059=DIRECTION('',(0.,0.,1.));
#20060=DIRECTION('',(-1.,1.92747052886312E-16,0.));
#20061=DIRECTION('center_axis',(0.707106781186551,0.707106781186544,0.));
#20062=DIRECTION('ref_axis',(-0.707106781186544,0.707106781186551,0.));
#20063=DIRECTION('',(-0.707106781186544,0.707106781186551,0.));
#20064=DIRECTION('',(0.,0.,1.));
#20065=DIRECTION('',(-0.707106781186544,0.707106781186551,0.));
#20066=DIRECTION('center_axis',(1.,0.,0.));
#20067=DIRECTION('ref_axis',(0.,0.,-1.));
#20068=DIRECTION('',(0.,1.,0.));
#20069=DIRECTION('',(0.,0.,1.));
#20070=DIRECTION('',(0.,1.,0.));
#20071=DIRECTION('center_axis',(0.707106781186546,-0.707106781186549,0.));
#20072=DIRECTION('ref_axis',(0.707106781186549,0.707106781186546,0.));
#20073=DIRECTION('',(0.707106781186549,0.707106781186546,0.));
#20074=DIRECTION('',(0.,0.,1.));
#20075=DIRECTION('',(0.707106781186549,0.707106781186546,0.));
#20076=DIRECTION('center_axis',(1.35393051783556E-15,-1.,0.));
#20077=DIRECTION('ref_axis',(1.,1.35393051783556E-15,0.));
#20078=DIRECTION('',(1.,1.35393051783556E-15,0.));
#20079=DIRECTION('',(1.,1.35393051783556E-15,0.));
#20080=DIRECTION('center_axis',(0.,0.,1.));
#20081=DIRECTION('ref_axis',(1.,0.,0.));
#20082=DIRECTION('center_axis',(0.,0.,1.));
#20083=DIRECTION('ref_axis',(1.,0.,0.));
#20084=DIRECTION('center_axis',(0.,0.886474799840877,0.462776867666349));
#20085=DIRECTION('ref_axis',(0.,-0.462776867666349,0.886474799840877));
#20086=DIRECTION('',(0.,-0.462776867666349,0.886474799840877));
#20087=DIRECTION('',(1.,0.,0.));
#20088=DIRECTION('',(0.,-0.462776867666349,0.886474799840877));
#20089=DIRECTION('',(1.,0.,0.));
#20090=DIRECTION('center_axis',(0.,1.,0.));
#20091=DIRECTION('ref_axis',(0.,0.,1.));
#20092=DIRECTION('',(0.,0.,1.));
#20093=DIRECTION('',(1.,0.,0.));
#20094=DIRECTION('',(0.,0.,1.));
#20095=DIRECTION('center_axis',(0.,0.707106781186542,-0.707106781186553));
#20096=DIRECTION('ref_axis',(0.,0.707106781186553,0.707106781186542));
#20097=DIRECTION('',(0.,0.707106781186553,0.707106781186542));
#20098=DIRECTION('',(1.,0.,0.));
#20099=DIRECTION('',(0.,0.707106781186553,0.707106781186542));
#20100=DIRECTION('center_axis',(0.,0.,-1.));
#20101=DIRECTION('ref_axis',(-1.,0.,0.));
#20102=DIRECTION('',(0.,1.,0.));
#20103=DIRECTION('',(1.,0.,0.));
#20104=DIRECTION('',(0.,1.,0.));
#20105=DIRECTION('center_axis',(0.,-0.707106781186547,-0.707106781186548));
#20106=DIRECTION('ref_axis',(0.,0.707106781186548,-0.707106781186547));
#20107=DIRECTION('',(0.,0.707106781186548,-0.707106781186547));
#20108=DIRECTION('',(1.,0.,0.));
#20109=DIRECTION('',(0.,0.707106781186548,-0.707106781186547));
#20110=DIRECTION('center_axis',(0.,-1.,0.));
#20111=DIRECTION('ref_axis',(0.,0.,-1.));
#20112=DIRECTION('',(0.,0.,-1.));
#20113=DIRECTION('',(1.,0.,0.));
#20114=DIRECTION('',(0.,0.,-1.));
#20115=DIRECTION('center_axis',(0.,0.,1.));
#20116=DIRECTION('ref_axis',(1.,0.,0.));
#20117=DIRECTION('',(0.,-1.,0.));
#20118=DIRECTION('',(0.,-1.,0.));
#20119=DIRECTION('center_axis',(-1.,0.,0.));
#20120=DIRECTION('ref_axis',(0.,0.,1.));
#20121=DIRECTION('center_axis',(-1.,0.,0.));
#20122=DIRECTION('ref_axis',(0.,0.,1.));
#20123=DIRECTION('center_axis',(0.,0.886474799840877,0.462776867666349));
#20124=DIRECTION('ref_axis',(0.,-0.462776867666349,0.886474799840877));
#20125=DIRECTION('',(0.,-0.462776867666349,0.886474799840877));
#20126=DIRECTION('',(1.,0.,0.));
#20127=DIRECTION('',(0.,-0.462776867666349,0.886474799840877));
#20128=DIRECTION('',(1.,0.,0.));
#20129=DIRECTION('center_axis',(0.,1.,0.));
#20130=DIRECTION('ref_axis',(0.,0.,1.));
#20131=DIRECTION('',(0.,0.,1.));
#20132=DIRECTION('',(1.,0.,0.));
#20133=DIRECTION('',(0.,0.,1.));
#20134=DIRECTION('center_axis',(0.,0.707106781186542,-0.707106781186553));
#20135=DIRECTION('ref_axis',(0.,0.707106781186553,0.707106781186542));
#20136=DIRECTION('',(0.,0.707106781186553,0.707106781186542));
#20137=DIRECTION('',(1.,0.,0.));
#20138=DIRECTION('',(0.,0.707106781186553,0.707106781186542));
#20139=DIRECTION('center_axis',(0.,0.,-1.));
#20140=DIRECTION('ref_axis',(-1.,0.,0.));
#20141=DIRECTION('',(0.,1.,0.));
#20142=DIRECTION('',(1.,0.,0.));
#20143=DIRECTION('',(0.,1.,0.));
#20144=DIRECTION('center_axis',(0.,-0.707106781186547,-0.707106781186548));
#20145=DIRECTION('ref_axis',(0.,0.707106781186548,-0.707106781186547));
#20146=DIRECTION('',(0.,0.707106781186548,-0.707106781186547));
#20147=DIRECTION('',(1.,0.,0.));
#20148=DIRECTION('',(0.,0.707106781186548,-0.707106781186547));
#20149=DIRECTION('center_axis',(0.,-1.,0.));
#20150=DIRECTION('ref_axis',(0.,0.,-1.));
#20151=DIRECTION('',(0.,0.,-1.));
#20152=DIRECTION('',(1.,0.,0.));
#20153=DIRECTION('',(0.,0.,-1.));
#20154=DIRECTION('center_axis',(0.,0.,1.));
#20155=DIRECTION('ref_axis',(1.,0.,0.));
#20156=DIRECTION('',(0.,-1.,0.));
#20157=DIRECTION('',(0.,-1.,0.));
#20158=DIRECTION('center_axis',(-1.,0.,0.));
#20159=DIRECTION('ref_axis',(0.,0.,1.));
#20160=DIRECTION('center_axis',(-1.,0.,0.));
#20161=DIRECTION('ref_axis',(0.,0.,1.));
#20162=DIRECTION('center_axis',(0.,0.886474799840877,0.462776867666349));
#20163=DIRECTION('ref_axis',(0.,-0.462776867666349,0.886474799840877));
#20164=DIRECTION('',(0.,-0.462776867666349,0.886474799840877));
#20165=DIRECTION('',(1.,0.,0.));
#20166=DIRECTION('',(0.,-0.462776867666349,0.886474799840877));
#20167=DIRECTION('',(1.,0.,0.));
#20168=DIRECTION('center_axis',(0.,1.,0.));
#20169=DIRECTION('ref_axis',(0.,0.,1.));
#20170=DIRECTION('',(0.,0.,1.));
#20171=DIRECTION('',(1.,0.,0.));
#20172=DIRECTION('',(0.,0.,1.));
#20173=DIRECTION('center_axis',(0.,0.707106781186542,-0.707106781186553));
#20174=DIRECTION('ref_axis',(0.,0.707106781186553,0.707106781186542));
#20175=DIRECTION('',(0.,0.707106781186553,0.707106781186542));
#20176=DIRECTION('',(1.,0.,0.));
#20177=DIRECTION('',(0.,0.707106781186553,0.707106781186542));
#20178=DIRECTION('center_axis',(0.,0.,-1.));
#20179=DIRECTION('ref_axis',(-1.,0.,0.));
#20180=DIRECTION('',(0.,1.,0.));
#20181=DIRECTION('',(1.,0.,0.));
#20182=DIRECTION('',(0.,1.,0.));
#20183=DIRECTION('center_axis',(0.,-0.707106781186547,-0.707106781186548));
#20184=DIRECTION('ref_axis',(0.,0.707106781186548,-0.707106781186547));
#20185=DIRECTION('',(0.,0.707106781186548,-0.707106781186547));
#20186=DIRECTION('',(1.,0.,0.));
#20187=DIRECTION('',(0.,0.707106781186548,-0.707106781186547));
#20188=DIRECTION('center_axis',(0.,-1.,0.));
#20189=DIRECTION('ref_axis',(0.,0.,-1.));
#20190=DIRECTION('',(0.,0.,-1.));
#20191=DIRECTION('',(1.,0.,0.));
#20192=DIRECTION('',(0.,0.,-1.));
#20193=DIRECTION('center_axis',(0.,0.,1.));
#20194=DIRECTION('ref_axis',(1.,0.,0.));
#20195=DIRECTION('',(0.,-1.,0.));
#20196=DIRECTION('',(0.,-1.,0.));
#20197=DIRECTION('center_axis',(-1.,0.,0.));
#20198=DIRECTION('ref_axis',(0.,0.,1.));
#20199=DIRECTION('center_axis',(-1.,0.,0.));
#20200=DIRECTION('ref_axis',(0.,0.,1.));
#20201=DIRECTION('center_axis',(0.,0.886474799840877,0.462776867666349));
#20202=DIRECTION('ref_axis',(0.,-0.462776867666349,0.886474799840877));
#20203=DIRECTION('',(0.,-0.462776867666349,0.886474799840877));
#20204=DIRECTION('',(-1.,0.,0.));
#20205=DIRECTION('',(0.,-0.462776867666349,0.886474799840877));
#20206=DIRECTION('',(-1.,0.,0.));
#20207=DIRECTION('center_axis',(0.,1.,0.));
#20208=DIRECTION('ref_axis',(0.,0.,1.));
#20209=DIRECTION('',(0.,0.,1.));
#20210=DIRECTION('',(0.,0.,1.));
#20211=DIRECTION('',(-1.,0.,0.));
#20212=DIRECTION('center_axis',(0.,0.707106781186542,-0.707106781186553));
#20213=DIRECTION('ref_axis',(0.,0.707106781186553,0.707106781186542));
#20214=DIRECTION('',(0.,0.707106781186553,0.707106781186542));
#20215=DIRECTION('',(0.,0.707106781186553,0.707106781186542));
#20216=DIRECTION('',(-1.,0.,0.));
#20217=DIRECTION('center_axis',(0.,0.,-1.));
#20218=DIRECTION('ref_axis',(1.,0.,0.));
#20219=DIRECTION('',(0.,1.,0.));
#20220=DIRECTION('',(0.,1.,0.));
#20221=DIRECTION('',(-1.,0.,0.));
#20222=DIRECTION('center_axis',(0.,-0.707106781186547,-0.707106781186548));
#20223=DIRECTION('ref_axis',(0.,0.707106781186548,-0.707106781186547));
#20224=DIRECTION('',(0.,0.707106781186548,-0.707106781186547));
#20225=DIRECTION('',(0.,0.707106781186548,-0.707106781186547));
#20226=DIRECTION('',(-1.,0.,0.));
#20227=DIRECTION('center_axis',(0.,-1.,0.));
#20228=DIRECTION('ref_axis',(0.,0.,-1.));
#20229=DIRECTION('',(0.,0.,-1.));
#20230=DIRECTION('',(0.,0.,-1.));
#20231=DIRECTION('',(-1.,0.,0.));
#20232=DIRECTION('center_axis',(0.,0.,1.));
#20233=DIRECTION('ref_axis',(-1.,0.,0.));
#20234=DIRECTION('',(0.,-1.,0.));
#20235=DIRECTION('',(0.,-1.,0.));
#20236=DIRECTION('center_axis',(1.,0.,0.));
#20237=DIRECTION('ref_axis',(0.,0.,1.));
#20238=DIRECTION('center_axis',(1.,0.,0.));
#20239=DIRECTION('ref_axis',(0.,0.,1.));
#20240=DIRECTION('center_axis',(0.,0.886474799840877,0.462776867666349));
#20241=DIRECTION('ref_axis',(0.,-0.462776867666349,0.886474799840877));
#20242=DIRECTION('',(0.,-0.462776867666349,0.886474799840877));
#20243=DIRECTION('',(-1.,0.,0.));
#20244=DIRECTION('',(0.,-0.462776867666349,0.886474799840877));
#20245=DIRECTION('',(-1.,0.,0.));
#20246=DIRECTION('center_axis',(0.,1.,0.));
#20247=DIRECTION('ref_axis',(0.,0.,1.));
#20248=DIRECTION('',(0.,0.,1.));
#20249=DIRECTION('',(0.,0.,1.));
#20250=DIRECTION('',(-1.,0.,0.));
#20251=DIRECTION('center_axis',(0.,0.707106781186542,-0.707106781186553));
#20252=DIRECTION('ref_axis',(0.,0.707106781186553,0.707106781186542));
#20253=DIRECTION('',(0.,0.707106781186553,0.707106781186542));
#20254=DIRECTION('',(0.,0.707106781186553,0.707106781186542));
#20255=DIRECTION('',(-1.,0.,0.));
#20256=DIRECTION('center_axis',(0.,0.,-1.));
#20257=DIRECTION('ref_axis',(1.,0.,0.));
#20258=DIRECTION('',(0.,1.,0.));
#20259=DIRECTION('',(0.,1.,0.));
#20260=DIRECTION('',(-1.,0.,0.));
#20261=DIRECTION('center_axis',(0.,-0.707106781186547,-0.707106781186548));
#20262=DIRECTION('ref_axis',(0.,0.707106781186548,-0.707106781186547));
#20263=DIRECTION('',(0.,0.707106781186548,-0.707106781186547));
#20264=DIRECTION('',(0.,0.707106781186548,-0.707106781186547));
#20265=DIRECTION('',(-1.,0.,0.));
#20266=DIRECTION('center_axis',(0.,-1.,0.));
#20267=DIRECTION('ref_axis',(0.,0.,-1.));
#20268=DIRECTION('',(0.,0.,-1.));
#20269=DIRECTION('',(0.,0.,-1.));
#20270=DIRECTION('',(-1.,0.,0.));
#20271=DIRECTION('center_axis',(0.,0.,1.));
#20272=DIRECTION('ref_axis',(-1.,0.,0.));
#20273=DIRECTION('',(0.,-1.,0.));
#20274=DIRECTION('',(0.,-1.,0.));
#20275=DIRECTION('center_axis',(1.,0.,0.));
#20276=DIRECTION('ref_axis',(0.,0.,1.));
#20277=DIRECTION('center_axis',(1.,0.,0.));
#20278=DIRECTION('ref_axis',(0.,0.,1.));
#20279=DIRECTION('center_axis',(0.400352069216121,-0.916361402872453,0.));
#20280=DIRECTION('ref_axis',(-0.916361402872453,-0.400352069216121,0.));
#20281=DIRECTION('',(-0.916361402872453,-0.400352069216121,0.));
#20282=DIRECTION('',(0.,0.,1.));
#20283=DIRECTION('',(-0.916361402872453,-0.400352069216121,0.));
#20284=DIRECTION('',(0.,0.,1.));
#20285=DIRECTION('center_axis',(1.,0.,0.));
#20286=DIRECTION('ref_axis',(0.,0.,1.));
#20287=DIRECTION('',(0.,-1.,0.));
#20288=DIRECTION('',(0.,-1.,0.));
#20289=DIRECTION('',(0.,0.,1.));
#20290=DIRECTION('center_axis',(-1.92747052886312E-16,1.,0.));
#20291=DIRECTION('ref_axis',(1.,1.92747052886312E-16,0.));
#20292=DIRECTION('',(1.,1.92747052886312E-16,0.));
#20293=DIRECTION('',(1.,1.92747052886312E-16,0.));
#20294=DIRECTION('',(0.,0.,1.));
#20295=DIRECTION('center_axis',(-0.707106781186551,0.707106781186544,0.));
#20296=DIRECTION('ref_axis',(0.707106781186544,0.707106781186551,0.));
#20297=DIRECTION('',(0.707106781186544,0.707106781186551,0.));
#20298=DIRECTION('',(0.707106781186544,0.707106781186551,0.));
#20299=DIRECTION('',(0.,0.,1.));
#20300=DIRECTION('center_axis',(-1.,0.,0.));
#20301=DIRECTION('ref_axis',(0.,0.,-1.));
#20302=DIRECTION('',(0.,1.,0.));
#20303=DIRECTION('',(0.,1.,0.));
#20304=DIRECTION('',(0.,0.,1.));
#20305=DIRECTION('center_axis',(-0.707106781186546,-0.707106781186549,0.));
#20306=DIRECTION('ref_axis',(-0.707106781186549,0.707106781186546,0.));
#20307=DIRECTION('',(-0.707106781186549,0.707106781186546,0.));
#20308=DIRECTION('',(-0.707106781186549,0.707106781186546,0.));
#20309=DIRECTION('',(0.,0.,1.));
#20310=DIRECTION('center_axis',(-1.35393051783556E-15,-1.,0.));
#20311=DIRECTION('ref_axis',(-1.,1.35393051783556E-15,0.));
#20312=DIRECTION('',(-1.,1.35393051783556E-15,0.));
#20313=DIRECTION('',(-1.,1.35393051783556E-15,0.));
#20314=DIRECTION('center_axis',(0.,0.,1.));
#20315=DIRECTION('ref_axis',(-1.,0.,0.));
#20316=DIRECTION('center_axis',(0.,0.,1.));
#20317=DIRECTION('ref_axis',(-1.,0.,0.));
#20318=DIRECTION('center_axis',(0.400352069216121,-0.916361402872453,0.));
#20319=DIRECTION('ref_axis',(-0.916361402872453,-0.400352069216121,0.));
#20320=DIRECTION('',(-0.916361402872453,-0.400352069216121,0.));
#20321=DIRECTION('',(0.,0.,1.));
#20322=DIRECTION('',(-0.916361402872453,-0.400352069216121,0.));
#20323=DIRECTION('',(0.,0.,1.));
#20324=DIRECTION('center_axis',(1.,0.,0.));
#20325=DIRECTION('ref_axis',(0.,0.,1.));
#20326=DIRECTION('',(0.,-1.,0.));
#20327=DIRECTION('',(0.,-1.,0.));
#20328=DIRECTION('',(0.,0.,1.));
#20329=DIRECTION('center_axis',(-1.92747052886312E-16,1.,0.));
#20330=DIRECTION('ref_axis',(1.,1.92747052886312E-16,0.));
#20331=DIRECTION('',(1.,1.92747052886312E-16,0.));
#20332=DIRECTION('',(1.,1.92747052886312E-16,0.));
#20333=DIRECTION('',(0.,0.,1.));
#20334=DIRECTION('center_axis',(-0.707106781186551,0.707106781186544,0.));
#20335=DIRECTION('ref_axis',(0.707106781186544,0.707106781186551,0.));
#20336=DIRECTION('',(0.707106781186544,0.707106781186551,0.));
#20337=DIRECTION('',(0.707106781186544,0.707106781186551,0.));
#20338=DIRECTION('',(0.,0.,1.));
#20339=DIRECTION('center_axis',(-1.,0.,0.));
#20340=DIRECTION('ref_axis',(0.,0.,-1.));
#20341=DIRECTION('',(0.,1.,0.));
#20342=DIRECTION('',(0.,1.,0.));
#20343=DIRECTION('',(0.,0.,1.));
#20344=DIRECTION('center_axis',(-0.707106781186546,-0.707106781186549,0.));
#20345=DIRECTION('ref_axis',(-0.707106781186549,0.707106781186546,0.));
#20346=DIRECTION('',(-0.707106781186549,0.707106781186546,0.));
#20347=DIRECTION('',(-0.707106781186549,0.707106781186546,0.));
#20348=DIRECTION('',(0.,0.,1.));
#20349=DIRECTION('center_axis',(-1.35393051783556E-15,-1.,0.));
#20350=DIRECTION('ref_axis',(-1.,1.35393051783556E-15,0.));
#20351=DIRECTION('',(-1.,1.35393051783556E-15,0.));
#20352=DIRECTION('',(-1.,1.35393051783556E-15,0.));
#20353=DIRECTION('center_axis',(0.,0.,1.));
#20354=DIRECTION('ref_axis',(-1.,0.,0.));
#20355=DIRECTION('center_axis',(0.,0.,1.));
#20356=DIRECTION('ref_axis',(-1.,0.,0.));
#20357=DIRECTION('center_axis',(0.400352069216121,-0.916361402872453,0.));
#20358=DIRECTION('ref_axis',(-0.916361402872453,-0.400352069216121,0.));
#20359=DIRECTION('',(-0.916361402872453,-0.400352069216121,0.));
#20360=DIRECTION('',(0.,0.,1.));
#20361=DIRECTION('',(-0.916361402872453,-0.400352069216121,0.));
#20362=DIRECTION('',(0.,0.,1.));
#20363=DIRECTION('center_axis',(1.,0.,0.));
#20364=DIRECTION('ref_axis',(0.,0.,1.));
#20365=DIRECTION('',(0.,-1.,0.));
#20366=DIRECTION('',(0.,-1.,0.));
#20367=DIRECTION('',(0.,0.,1.));
#20368=DIRECTION('center_axis',(-1.92747052886312E-16,1.,0.));
#20369=DIRECTION('ref_axis',(1.,1.92747052886312E-16,0.));
#20370=DIRECTION('',(1.,1.92747052886312E-16,0.));
#20371=DIRECTION('',(1.,1.92747052886312E-16,0.));
#20372=DIRECTION('',(0.,0.,1.));
#20373=DIRECTION('center_axis',(-0.707106781186551,0.707106781186544,0.));
#20374=DIRECTION('ref_axis',(0.707106781186544,0.707106781186551,0.));
#20375=DIRECTION('',(0.707106781186544,0.707106781186551,0.));
#20376=DIRECTION('',(0.707106781186544,0.707106781186551,0.));
#20377=DIRECTION('',(0.,0.,1.));
#20378=DIRECTION('center_axis',(-1.,0.,0.));
#20379=DIRECTION('ref_axis',(0.,0.,-1.));
#20380=DIRECTION('',(0.,1.,0.));
#20381=DIRECTION('',(0.,1.,0.));
#20382=DIRECTION('',(0.,0.,1.));
#20383=DIRECTION('center_axis',(-0.707106781186546,-0.707106781186549,0.));
#20384=DIRECTION('ref_axis',(-0.707106781186549,0.707106781186546,0.));
#20385=DIRECTION('',(-0.707106781186549,0.707106781186546,0.));
#20386=DIRECTION('',(-0.707106781186549,0.707106781186546,0.));
#20387=DIRECTION('',(0.,0.,1.));
#20388=DIRECTION('center_axis',(-1.35393051783556E-15,-1.,0.));
#20389=DIRECTION('ref_axis',(-1.,1.35393051783556E-15,0.));
#20390=DIRECTION('',(-1.,1.35393051783556E-15,0.));
#20391=DIRECTION('',(-1.,1.35393051783556E-15,0.));
#20392=DIRECTION('center_axis',(0.,0.,1.));
#20393=DIRECTION('ref_axis',(-1.,0.,0.));
#20394=DIRECTION('center_axis',(0.,0.,1.));
#20395=DIRECTION('ref_axis',(-1.,0.,0.));
#20396=DIRECTION('center_axis',(0.,1.,0.));
#20397=DIRECTION('ref_axis',(0.,0.,1.));
#20398=DIRECTION('center_axis',(0.,1.,0.));
#20399=DIRECTION('ref_axis',(0.,0.,-1.));
#20400=DIRECTION('',(0.,1.,0.));
#20401=DIRECTION('center_axis',(0.,1.,0.));
#20402=DIRECTION('ref_axis',(0.,0.,-1.));
#20403=DIRECTION('center_axis',(0.,1.,0.));
#20404=DIRECTION('ref_axis',(0.,0.,1.));
#20405=DIRECTION('center_axis',(0.,1.,0.));
#20406=DIRECTION('ref_axis',(0.,0.,-1.));
#20407=DIRECTION('',(0.,1.,0.));
#20408=DIRECTION('center_axis',(0.,1.,0.));
#20409=DIRECTION('ref_axis',(0.,0.,-1.));
#20410=DIRECTION('center_axis',(0.,1.,0.));
#20411=DIRECTION('ref_axis',(0.,0.,1.));
#20412=DIRECTION('center_axis',(0.,1.,0.));
#20413=DIRECTION('ref_axis',(0.,0.,-1.));
#20414=DIRECTION('',(0.,1.,0.));
#20415=DIRECTION('center_axis',(0.,1.,0.));
#20416=DIRECTION('ref_axis',(0.,0.,-1.));
#20417=DIRECTION('center_axis',(0.,1.,0.));
#20418=DIRECTION('ref_axis',(0.,0.,1.));
#20419=DIRECTION('center_axis',(0.,1.,0.));
#20420=DIRECTION('ref_axis',(0.,0.,-1.));
#20421=DIRECTION('',(0.,1.,0.));
#20422=DIRECTION('center_axis',(0.,1.,0.));
#20423=DIRECTION('ref_axis',(0.,0.,-1.));
#20424=DIRECTION('center_axis',(0.,1.,0.));
#20425=DIRECTION('ref_axis',(0.,0.,1.));
#20426=DIRECTION('',(-2.36721327212187E-16,0.,-1.));
#20427=DIRECTION('',(1.,0.,-1.13752359080446E-16));
#20428=DIRECTION('',(2.36721327212187E-16,0.,1.));
#20429=DIRECTION('',(-1.,0.,-3.03339624214524E-16));
#20430=DIRECTION('center_axis',(0.,1.,0.));
#20431=DIRECTION('ref_axis',(0.,0.,1.));
#20432=DIRECTION('',(-2.36721327212187E-16,0.,-1.));
#20433=DIRECTION('',(-1.,0.,-3.03339624214524E-16));
#20434=DIRECTION('',(2.36721327212187E-16,0.,1.));
#20435=DIRECTION('',(1.,0.,-1.13752359080446E-16));
#20436=DIRECTION('center_axis',(-1.,0.,2.36721327212187E-16));
#20437=DIRECTION('ref_axis',(-2.36721327212187E-16,0.,-1.));
#20438=DIRECTION('',(0.,1.,0.));
#20439=DIRECTION('',(0.,1.,0.));
#20440=DIRECTION('center_axis',(-3.03339624214524E-16,0.,1.));
#20441=DIRECTION('ref_axis',(-1.,0.,-3.03339624214524E-16));
#20442=DIRECTION('',(0.,1.,0.));
#20443=DIRECTION('center_axis',(1.,0.,-2.36721327212187E-16));
#20444=DIRECTION('ref_axis',(2.36721327212187E-16,0.,1.));
#20445=DIRECTION('',(0.,1.,0.));
#20446=DIRECTION('center_axis',(-1.13752359080446E-16,0.,-1.));
#20447=DIRECTION('ref_axis',(1.,0.,-1.13752359080446E-16));
#20448=DIRECTION('center_axis',(1.,1.23267486838602E-16,-7.11670202791209E-17));
#20449=DIRECTION('ref_axis',(-1.23267486838602E-16,1.,6.0466247699241E-49));
#20450=DIRECTION('',(1.42336285208353E-16,-0.866029956157432,0.499992114975783));
#20451=DIRECTION('',(0.,-0.499992114975783,-0.866029956157432));
#20452=DIRECTION('',(1.42336285208353E-16,-0.866029956157432,0.499992114975783));
#20453=DIRECTION('',(0.,-0.499992114975783,-0.866029956157432));
#20454=DIRECTION('center_axis',(0.,0.866029956157432,-0.499992114975783));
#20455=DIRECTION('ref_axis',(0.,0.499992114975783,0.866029956157432));
#20456=DIRECTION('',(1.,0.,0.));
#20457=DIRECTION('',(0.,-0.499992114975783,-0.866029956157432));
#20458=DIRECTION('',(1.,0.,0.));
#20459=DIRECTION('center_axis',(-1.,0.,0.));
#20460=DIRECTION('ref_axis',(0.,0.,1.));
#20461=DIRECTION('',(0.,0.866029956157432,-0.499992114975783));
#20462=DIRECTION('',(0.,-0.499992114975783,-0.866029956157432));
#20463=DIRECTION('',(0.,0.866029956157432,-0.499992114975783));
#20464=DIRECTION('center_axis',(0.,-0.866029956157432,0.499992114975783));
#20465=DIRECTION('ref_axis',(0.,-0.499992114975783,-0.866029956157432));
#20466=DIRECTION('',(-1.,0.,0.));
#20467=DIRECTION('',(-1.,0.,0.));
#20468=DIRECTION('center_axis',(0.,0.499992114975783,0.866029956157432));
#20469=DIRECTION('ref_axis',(0.,-0.866029956157432,0.499992114975783));
#20470=DIRECTION('center_axis',(0.,0.499992114975783,0.866029956157432));
#20471=DIRECTION('ref_axis',(0.,-0.866029956157432,0.499992114975783));
#20472=DIRECTION('center_axis',(1.,-7.11113466337029E-16,4.10552918514724E-16));
#20473=DIRECTION('ref_axis',(7.1111346633703E-16,1.,8.60465311718737E-48));
#20474=DIRECTION('',(-8.21118786112474E-16,-0.866029956157432,0.499992114975783));
#20475=DIRECTION('',(0.,-0.499992114975783,-0.866029956157432));
#20476=DIRECTION('',(-8.21118786112474E-16,-0.866029956157432,0.499992114975783));
#20477=DIRECTION('',(0.,-0.499992114975783,-0.866029956157432));
#20478=DIRECTION('center_axis',(0.,0.866029956157432,-0.499992114975783));
#20479=DIRECTION('ref_axis',(0.,0.499992114975783,0.866029956157432));
#20480=DIRECTION('',(1.,0.,0.));
#20481=DIRECTION('',(0.,-0.499992114975783,-0.866029956157432));
#20482=DIRECTION('',(1.,0.,0.));
#20483=DIRECTION('center_axis',(-1.,0.,0.));
#20484=DIRECTION('ref_axis',(0.,0.,1.));
#20485=DIRECTION('',(0.,0.866029956157432,-0.499992114975783));
#20486=DIRECTION('',(0.,-0.499992114975783,-0.866029956157432));
#20487=DIRECTION('',(0.,0.866029956157432,-0.499992114975783));
#20488=DIRECTION('center_axis',(0.,-0.866029956157432,0.499992114975783));
#20489=DIRECTION('ref_axis',(0.,-0.499992114975783,-0.866029956157432));
#20490=DIRECTION('',(-1.,0.,0.));
#20491=DIRECTION('',(-1.,0.,0.));
#20492=DIRECTION('center_axis',(0.,0.499992114975783,0.866029956157432));
#20493=DIRECTION('ref_axis',(0.,-0.866029956157432,0.499992114975783));
#20494=DIRECTION('center_axis',(0.,0.499992114975783,0.866029956157432));
#20495=DIRECTION('ref_axis',(0.,-0.866029956157432,0.499992114975783));
#20496=DIRECTION('center_axis',(1.,0.,0.));
#20497=DIRECTION('ref_axis',(0.,0.,-1.));
#20498=DIRECTION('',(0.,-0.866029956157432,0.499992114975783));
#20499=DIRECTION('',(0.,-0.499992114975783,-0.866029956157432));
#20500=DIRECTION('',(0.,-0.866029956157432,0.499992114975783));
#20501=DIRECTION('',(0.,-0.499992114975783,-0.866029956157432));
#20502=DIRECTION('center_axis',(0.,0.866029956157432,-0.499992114975783));
#20503=DIRECTION('ref_axis',(0.,0.499992114975783,0.866029956157432));
#20504=DIRECTION('',(1.,0.,0.));
#20505=DIRECTION('',(0.,-0.499992114975783,-0.866029956157432));
#20506=DIRECTION('',(1.,0.,0.));
#20507=DIRECTION('center_axis',(-1.,0.,0.));
#20508=DIRECTION('ref_axis',(0.,0.,1.));
#20509=DIRECTION('',(0.,0.866029956157432,-0.499992114975783));
#20510=DIRECTION('',(0.,-0.499992114975783,-0.866029956157432));
#20511=DIRECTION('',(0.,0.866029956157432,-0.499992114975783));
#20512=DIRECTION('center_axis',(0.,-0.866029956157432,0.499992114975783));
#20513=DIRECTION('ref_axis',(0.,-0.499992114975783,-0.866029956157432));
#20514=DIRECTION('',(-1.,0.,0.));
#20515=DIRECTION('',(-1.,0.,0.));
#20516=DIRECTION('center_axis',(0.,0.499992114975783,0.866029956157432));
#20517=DIRECTION('ref_axis',(0.,-0.866029956157432,0.499992114975783));
#20518=DIRECTION('center_axis',(0.,0.499992114975783,0.866029956157432));
#20519=DIRECTION('ref_axis',(0.,-0.866029956157432,0.499992114975783));
#20520=DIRECTION('center_axis',(1.,0.,0.));
#20521=DIRECTION('ref_axis',(0.,0.,-1.));
#20522=DIRECTION('',(0.,-0.866029956157432,0.499992114975783));
#20523=DIRECTION('',(0.,-0.499992114975783,-0.866029956157432));
#20524=DIRECTION('',(0.,-0.866029956157432,0.499992114975783));
#20525=DIRECTION('',(0.,-0.499992114975783,-0.866029956157432));
#20526=DIRECTION('center_axis',(0.,0.866029956157432,-0.499992114975783));
#20527=DIRECTION('ref_axis',(0.,0.499992114975783,0.866029956157432));
#20528=DIRECTION('',(1.,0.,0.));
#20529=DIRECTION('',(0.,-0.499992114975783,-0.866029956157432));
#20530=DIRECTION('',(1.,0.,0.));
#20531=DIRECTION('center_axis',(-1.,0.,0.));
#20532=DIRECTION('ref_axis',(0.,0.,1.));
#20533=DIRECTION('',(0.,0.866029956157432,-0.499992114975783));
#20534=DIRECTION('',(0.,-0.499992114975783,-0.866029956157432));
#20535=DIRECTION('',(0.,0.866029956157432,-0.499992114975783));
#20536=DIRECTION('center_axis',(0.,-0.866029956157432,0.499992114975783));
#20537=DIRECTION('ref_axis',(0.,-0.499992114975783,-0.866029956157432));
#20538=DIRECTION('',(-1.,0.,0.));
#20539=DIRECTION('',(-1.,0.,0.));
#20540=DIRECTION('center_axis',(0.,0.499992114975783,0.866029956157432));
#20541=DIRECTION('ref_axis',(0.,-0.866029956157432,0.499992114975783));
#20542=DIRECTION('center_axis',(0.,0.499992114975783,0.866029956157432));
#20543=DIRECTION('ref_axis',(0.,-0.866029956157432,0.499992114975783));
#20544=DIRECTION('center_axis',(1.,0.,0.));
#20545=DIRECTION('ref_axis',(0.,0.,-1.));
#20546=DIRECTION('',(0.,-0.866029956157432,0.499992114975783));
#20547=DIRECTION('',(0.,-0.499992114975783,-0.866029956157432));
#20548=DIRECTION('',(0.,-0.866029956157432,0.499992114975783));
#20549=DIRECTION('',(0.,-0.499992114975783,-0.866029956157432));
#20550=DIRECTION('center_axis',(0.,0.866029956157432,-0.499992114975783));
#20551=DIRECTION('ref_axis',(0.,0.499992114975783,0.866029956157432));
#20552=DIRECTION('',(1.,0.,0.));
#20553=DIRECTION('',(0.,-0.499992114975783,-0.866029956157432));
#20554=DIRECTION('',(1.,0.,0.));
#20555=DIRECTION('center_axis',(-1.,0.,0.));
#20556=DIRECTION('ref_axis',(0.,0.,1.));
#20557=DIRECTION('',(0.,0.866029956157432,-0.499992114975783));
#20558=DIRECTION('',(0.,-0.499992114975783,-0.866029956157432));
#20559=DIRECTION('',(0.,0.866029956157432,-0.499992114975783));
#20560=DIRECTION('center_axis',(0.,-0.866029956157432,0.499992114975783));
#20561=DIRECTION('ref_axis',(0.,-0.499992114975783,-0.866029956157432));
#20562=DIRECTION('',(-1.,0.,0.));
#20563=DIRECTION('',(-1.,0.,0.));
#20564=DIRECTION('center_axis',(0.,0.499992114975783,0.866029956157432));
#20565=DIRECTION('ref_axis',(0.,-0.866029956157432,0.499992114975783));
#20566=DIRECTION('center_axis',(0.,0.499992114975783,0.866029956157432));
#20567=DIRECTION('ref_axis',(0.,-0.866029956157432,0.499992114975783));
#20568=DIRECTION('center_axis',(1.,-3.55556733168515E-16,2.05276459257362E-16));
#20569=DIRECTION('ref_axis',(3.55556733168515E-16,1.,2.15116327929684E-48));
#20570=DIRECTION('',(-4.10559393056237E-16,-0.866029956157432,0.499992114975783));
#20571=DIRECTION('',(0.,-0.499992114975783,-0.866029956157432));
#20572=DIRECTION('',(-4.10559393056237E-16,-0.866029956157432,0.499992114975783));
#20573=DIRECTION('',(0.,-0.499992114975783,-0.866029956157432));
#20574=DIRECTION('center_axis',(0.,0.866029956157432,-0.499992114975783));
#20575=DIRECTION('ref_axis',(0.,0.499992114975783,0.866029956157432));
#20576=DIRECTION('',(1.,0.,0.));
#20577=DIRECTION('',(0.,-0.499992114975783,-0.866029956157432));
#20578=DIRECTION('',(1.,0.,0.));
#20579=DIRECTION('center_axis',(-1.,7.16669040292788E-16,-4.1376036319062E-16));
#20580=DIRECTION('ref_axis',(-7.16669040292788E-16,-1.,2.01352657371916E-47));
#20581=DIRECTION('',(8.27533776628978E-16,0.866029956157432,-0.499992114975783));
#20582=DIRECTION('',(0.,-0.499992114975783,-0.866029956157432));
#20583=DIRECTION('',(8.27533776628978E-16,0.866029956157432,-0.499992114975783));
#20584=DIRECTION('center_axis',(0.,-0.866029956157432,0.499992114975783));
#20585=DIRECTION('ref_axis',(0.,-0.499992114975783,-0.866029956157432));
#20586=DIRECTION('',(-1.,0.,0.));
#20587=DIRECTION('',(-1.,0.,0.));
#20588=DIRECTION('center_axis',(0.,0.499992114975783,0.866029956157432));
#20589=DIRECTION('ref_axis',(0.,-0.866029956157432,0.499992114975783));
#20590=DIRECTION('center_axis',(0.,0.499992114975783,0.866029956157432));
#20591=DIRECTION('ref_axis',(0.,-0.866029956157432,0.499992114975783));
#20592=DIRECTION('center_axis',(1.67968331250372E-16,-0.866029956157432,
0.499992114975783));
#20593=DIRECTION('ref_axis',(-5.57351334278697E-33,-0.499992114975783,-0.866029956157432));
#20594=DIRECTION('',(-1.,-1.50505749146232E-16,7.52528745731158E-17));
#20595=DIRECTION('',(0.,-0.499992114975783,-0.866029956157432));
#20596=DIRECTION('',(-1.,-1.50505749146232E-16,7.52528745731158E-17));
#20597=DIRECTION('',(0.,-0.499992114975783,-0.866029956157432));
#20598=DIRECTION('center_axis',(0.866185586048601,0.432774614486462,-0.249857286421141));
#20599=DIRECTION('ref_axis',(-0.446950695480887,0.894558592719981,-6.35609056424636E-18));
#20600=DIRECTION('',(0.499722453489576,-0.750142665109869,0.433085963129978));
#20601=DIRECTION('',(0.,-0.499992114975783,-0.866029956157432));
#20602=DIRECTION('',(0.499722453489576,-0.750142665109869,0.433085963129978));
#20603=DIRECTION('center_axis',(0.,0.866029956157432,-0.499992114975783));
#20604=DIRECTION('ref_axis',(0.,0.499992114975783,0.866029956157432));
#20605=DIRECTION('',(1.,0.,0.));
#20606=DIRECTION('',(0.,-0.499992114975783,-0.866029956157432));
#20607=DIRECTION('',(1.,0.,0.));
#20608=DIRECTION('center_axis',(-0.866185586048601,0.432774614486462,-0.249857286421141));
#20609=DIRECTION('ref_axis',(-0.446950695480887,-0.89455859271998,8.76410190439018E-18));
#20610=DIRECTION('',(0.499722453489577,0.750142665109869,-0.433085963129978));
#20611=DIRECTION('',(0.499722453489577,0.750142665109869,-0.433085963129978));
#20612=DIRECTION('center_axis',(-1.00804441643628E-17,0.499992114975783,
0.866029956157432));
#20613=DIRECTION('ref_axis',(6.68767698777501E-35,-0.866029956157432,0.499992114975783));
#20614=DIRECTION('center_axis',(-1.00804441643628E-17,0.499992114975783,
0.866029956157432));
#20615=DIRECTION('ref_axis',(6.68767698777501E-35,-0.866029956157432,0.499992114975783));
#20616=DIRECTION('center_axis',(3.0024060161137E-16,0.499992114975783,0.866029956157432));
#20617=DIRECTION('ref_axis',(-1.13450604310479E-33,-0.866029956157432,0.499992114975783));
#20618=DIRECTION('',(-0.499722453489577,-0.750142665109869,0.433085963129978));
#20619=DIRECTION('',(0.866185586048601,-0.432774614486463,0.249857286421141));
#20620=DIRECTION('',(-0.499722453489577,-0.750142665109869,0.433085963129978));
#20621=DIRECTION('',(0.866185586048601,-0.432774614486463,0.249857286421141));
#20622=DIRECTION('center_axis',(0.499722453489577,0.750142665109869,-0.433085963129978));
#20623=DIRECTION('ref_axis',(-0.832241064261676,0.554413934670291,-3.58035061299401E-18));
#20624=DIRECTION('',(0.,0.499992114975783,0.866029956157432));
#20625=DIRECTION('',(0.866185586048601,-0.432774614486463,0.249857286421141));
#20626=DIRECTION('',(0.,0.499992114975783,0.866029956157432));
#20627=DIRECTION('center_axis',(0.,-0.499992114975783,-0.866029956157432));
#20628=DIRECTION('ref_axis',(0.,0.866029956157432,-0.499992114975783));
#20629=DIRECTION('',(0.499722453489577,0.750142665109869,-0.433085963129978));
#20630=DIRECTION('',(0.866185586048601,-0.432774614486463,0.249857286421141));
#20631=DIRECTION('',(0.499722453489577,0.750142665109869,-0.433085963129978));
#20632=DIRECTION('center_axis',(-0.499722453489577,-0.750142665109869,0.433085963129978));
#20633=DIRECTION('ref_axis',(0.832241064261676,-0.554413934670291,3.58035061299401E-18));
#20634=DIRECTION('',(0.,-0.499992114975783,-0.866029956157432));
#20635=DIRECTION('',(0.,-0.499992114975783,-0.866029956157432));
#20636=DIRECTION('center_axis',(-0.866185586048601,0.432774614486463,-0.249857286421141));
#20637=DIRECTION('ref_axis',(-0.446950695480888,-0.89455859271998,1.05171903626344E-18));
#20638=DIRECTION('center_axis',(-0.866185586048601,0.432774614486463,-0.249857286421141));
#20639=DIRECTION('ref_axis',(-0.446950695480888,-0.89455859271998,1.05171903626344E-18));
#20640=DIRECTION('center_axis',(3.0024060161137E-16,0.499992114975783,0.866029956157432));
#20641=DIRECTION('ref_axis',(-1.13450604310479E-33,-0.866029956157432,0.499992114975783));
#20642=DIRECTION('',(-0.499722453489577,-0.750142665109869,0.433085963129978));
#20643=DIRECTION('',(0.866185586048601,-0.432774614486463,0.249857286421141));
#20644=DIRECTION('',(-0.499722453489577,-0.750142665109869,0.433085963129978));
#20645=DIRECTION('',(0.866185586048601,-0.432774614486463,0.249857286421141));
#20646=DIRECTION('center_axis',(0.499722453489577,0.750142665109869,-0.433085963129978));
#20647=DIRECTION('ref_axis',(-0.832241064261676,0.554413934670291,-3.58035061299401E-18));
#20648=DIRECTION('',(0.,0.499992114975783,0.866029956157432));
#20649=DIRECTION('',(0.866185586048601,-0.432774614486463,0.249857286421141));
#20650=DIRECTION('',(0.,0.499992114975783,0.866029956157432));
#20651=DIRECTION('center_axis',(0.,-0.499992114975783,-0.866029956157432));
#20652=DIRECTION('ref_axis',(0.,0.866029956157432,-0.499992114975783));
#20653=DIRECTION('',(0.499722453489577,0.750142665109869,-0.433085963129978));
#20654=DIRECTION('',(0.866185586048601,-0.432774614486463,0.249857286421141));
#20655=DIRECTION('',(0.499722453489577,0.750142665109869,-0.433085963129978));
#20656=DIRECTION('center_axis',(-0.499722453489577,-0.750142665109869,0.433085963129978));
#20657=DIRECTION('ref_axis',(0.832241064261676,-0.554413934670291,3.58035061299401E-18));
#20658=DIRECTION('',(0.,-0.499992114975783,-0.866029956157432));
#20659=DIRECTION('',(0.,-0.499992114975783,-0.866029956157432));
#20660=DIRECTION('center_axis',(-0.866185586048601,0.432774614486463,-0.249857286421141));
#20661=DIRECTION('ref_axis',(-0.446950695480888,-0.89455859271998,1.05171903626344E-18));
#20662=DIRECTION('center_axis',(-0.866185586048601,0.432774614486463,-0.249857286421141));
#20663=DIRECTION('ref_axis',(-0.446950695480888,-0.89455859271998,1.05171903626344E-18));
#20664=DIRECTION('center_axis',(3.0024060161137E-16,0.499992114975783,0.866029956157432));
#20665=DIRECTION('ref_axis',(-1.13450604310479E-33,-0.866029956157432,0.499992114975783));
#20666=DIRECTION('',(-0.499722453489577,-0.750142665109869,0.433085963129978));
#20667=DIRECTION('',(0.866185586048601,-0.432774614486463,0.249857286421141));
#20668=DIRECTION('',(-0.499722453489577,-0.750142665109869,0.433085963129978));
#20669=DIRECTION('',(0.866185586048601,-0.432774614486463,0.249857286421141));
#20670=DIRECTION('center_axis',(0.499722453489577,0.750142665109869,-0.433085963129978));
#20671=DIRECTION('ref_axis',(-0.832241064261676,0.554413934670291,-3.58035061299401E-18));
#20672=DIRECTION('',(0.,0.499992114975783,0.866029956157432));
#20673=DIRECTION('',(0.866185586048601,-0.432774614486463,0.249857286421141));
#20674=DIRECTION('',(0.,0.499992114975783,0.866029956157432));
#20675=DIRECTION('center_axis',(0.,-0.499992114975783,-0.866029956157432));
#20676=DIRECTION('ref_axis',(0.,0.866029956157432,-0.499992114975783));
#20677=DIRECTION('',(0.499722453489577,0.750142665109869,-0.433085963129978));
#20678=DIRECTION('',(0.866185586048601,-0.432774614486463,0.249857286421141));
#20679=DIRECTION('',(0.499722453489577,0.750142665109869,-0.433085963129978));
#20680=DIRECTION('center_axis',(-0.499722453489577,-0.750142665109869,0.433085963129978));
#20681=DIRECTION('ref_axis',(0.832241064261676,-0.554413934670291,3.58035061299401E-18));
#20682=DIRECTION('',(0.,-0.499992114975783,-0.866029956157432));
#20683=DIRECTION('',(0.,-0.499992114975783,-0.866029956157432));
#20684=DIRECTION('center_axis',(-0.866185586048601,0.432774614486463,-0.249857286421141));
#20685=DIRECTION('ref_axis',(-0.446950695480888,-0.89455859271998,1.05171903626344E-18));
#20686=DIRECTION('center_axis',(-0.866185586048601,0.432774614486463,-0.249857286421141));
#20687=DIRECTION('ref_axis',(-0.446950695480888,-0.89455859271998,1.05171903626344E-18));
#20688=DIRECTION('center_axis',(3.0024060161137E-16,0.499992114975783,0.866029956157432));
#20689=DIRECTION('ref_axis',(-1.13450604310479E-33,-0.866029956157432,0.499992114975783));
#20690=DIRECTION('',(-0.499722453489577,-0.750142665109869,0.433085963129978));
#20691=DIRECTION('',(0.866185586048601,-0.432774614486463,0.249857286421141));
#20692=DIRECTION('',(-0.499722453489577,-0.750142665109869,0.433085963129978));
#20693=DIRECTION('',(0.866185586048601,-0.432774614486463,0.249857286421141));
#20694=DIRECTION('center_axis',(0.499722453489577,0.750142665109869,-0.433085963129978));
#20695=DIRECTION('ref_axis',(-0.832241064261676,0.554413934670291,-3.58035061299401E-18));
#20696=DIRECTION('',(0.,0.499992114975783,0.866029956157432));
#20697=DIRECTION('',(0.866185586048601,-0.432774614486463,0.249857286421141));
#20698=DIRECTION('',(0.,0.499992114975783,0.866029956157432));
#20699=DIRECTION('center_axis',(0.,-0.499992114975783,-0.866029956157432));
#20700=DIRECTION('ref_axis',(0.,0.866029956157432,-0.499992114975783));
#20701=DIRECTION('',(0.499722453489577,0.750142665109869,-0.433085963129978));
#20702=DIRECTION('',(0.866185586048601,-0.432774614486463,0.249857286421141));
#20703=DIRECTION('',(0.499722453489577,0.750142665109869,-0.433085963129978));
#20704=DIRECTION('center_axis',(-0.499722453489577,-0.750142665109869,0.433085963129978));
#20705=DIRECTION('ref_axis',(0.832241064261676,-0.554413934670291,3.58035061299401E-18));
#20706=DIRECTION('',(0.,-0.499992114975783,-0.866029956157432));
#20707=DIRECTION('',(0.,-0.499992114975783,-0.866029956157432));
#20708=DIRECTION('center_axis',(-0.866185586048601,0.432774614486463,-0.249857286421141));
#20709=DIRECTION('ref_axis',(-0.446950695480888,-0.89455859271998,1.05171903626344E-18));
#20710=DIRECTION('center_axis',(-0.866185586048601,0.432774614486463,-0.249857286421141));
#20711=DIRECTION('ref_axis',(-0.446950695480888,-0.89455859271998,1.05171903626344E-18));
#20712=DIRECTION('center_axis',(-3.0024060161137E-16,0.499992114975783,
0.866029956157432));
#20713=DIRECTION('ref_axis',(1.13450604310479E-33,-0.866029956157432,0.499992114975783));
#20714=DIRECTION('',(0.499722453489577,-0.750142665109869,0.433085963129978));
#20715=DIRECTION('',(-0.866185586048601,-0.432774614486463,0.249857286421141));
#20716=DIRECTION('',(0.499722453489577,-0.750142665109869,0.433085963129978));
#20717=DIRECTION('',(-0.866185586048601,-0.432774614486463,0.249857286421141));
#20718=DIRECTION('center_axis',(-0.499722453489577,0.750142665109869,-0.433085963129978));
#20719=DIRECTION('ref_axis',(0.832241064261676,0.554413934670291,-3.58035061299401E-18));
#20720=DIRECTION('',(0.,0.499992114975783,0.866029956157432));
#20721=DIRECTION('',(0.,0.499992114975783,0.866029956157432));
#20722=DIRECTION('',(-0.866185586048601,-0.432774614486463,0.249857286421141));
#20723=DIRECTION('center_axis',(0.,-0.499992114975783,-0.866029956157432));
#20724=DIRECTION('ref_axis',(0.,0.866029956157432,-0.499992114975783));
#20725=DIRECTION('',(-0.499722453489577,0.750142665109869,-0.433085963129978));
#20726=DIRECTION('',(-0.499722453489577,0.750142665109869,-0.433085963129978));
#20727=DIRECTION('',(-0.866185586048601,-0.432774614486463,0.249857286421141));
#20728=DIRECTION('center_axis',(0.499722453489577,-0.750142665109869,0.433085963129978));
#20729=DIRECTION('ref_axis',(-0.832241064261676,-0.554413934670291,3.58035061299401E-18));
#20730=DIRECTION('',(0.,-0.499992114975783,-0.866029956157432));
#20731=DIRECTION('',(0.,-0.499992114975783,-0.866029956157432));
#20732=DIRECTION('center_axis',(0.866185586048601,0.432774614486463,-0.249857286421141));
#20733=DIRECTION('ref_axis',(0.446950695480888,-0.89455859271998,1.05171903626344E-18));
#20734=DIRECTION('center_axis',(0.866185586048601,0.432774614486463,-0.249857286421141));
#20735=DIRECTION('ref_axis',(0.446950695480888,-0.89455859271998,1.05171903626344E-18));
#20736=DIRECTION('center_axis',(-3.0024060161137E-16,0.499992114975783,
0.866029956157432));
#20737=DIRECTION('ref_axis',(1.13450604310479E-33,-0.866029956157432,0.499992114975783));
#20738=DIRECTION('',(0.499722453489577,-0.750142665109869,0.433085963129978));
#20739=DIRECTION('',(-0.866185586048601,-0.432774614486463,0.249857286421141));
#20740=DIRECTION('',(0.499722453489577,-0.750142665109869,0.433085963129978));
#20741=DIRECTION('',(-0.866185586048601,-0.432774614486463,0.249857286421141));
#20742=DIRECTION('center_axis',(-0.499722453489577,0.750142665109869,-0.433085963129978));
#20743=DIRECTION('ref_axis',(0.832241064261676,0.554413934670291,-3.58035061299401E-18));
#20744=DIRECTION('',(0.,0.499992114975783,0.866029956157432));
#20745=DIRECTION('',(0.,0.499992114975783,0.866029956157432));
#20746=DIRECTION('',(-0.866185586048601,-0.432774614486463,0.249857286421141));
#20747=DIRECTION('center_axis',(0.,-0.499992114975783,-0.866029956157432));
#20748=DIRECTION('ref_axis',(0.,0.866029956157432,-0.499992114975783));
#20749=DIRECTION('',(-0.499722453489577,0.750142665109869,-0.433085963129978));
#20750=DIRECTION('',(-0.499722453489577,0.750142665109869,-0.433085963129978));
#20751=DIRECTION('',(-0.866185586048601,-0.432774614486463,0.249857286421141));
#20752=DIRECTION('center_axis',(0.499722453489577,-0.750142665109869,0.433085963129978));
#20753=DIRECTION('ref_axis',(-0.832241064261676,-0.554413934670291,3.58035061299401E-18));
#20754=DIRECTION('',(0.,-0.499992114975783,-0.866029956157432));
#20755=DIRECTION('',(0.,-0.499992114975783,-0.866029956157432));
#20756=DIRECTION('center_axis',(0.866185586048601,0.432774614486463,-0.249857286421141));
#20757=DIRECTION('ref_axis',(0.446950695480888,-0.89455859271998,1.05171903626344E-18));
#20758=DIRECTION('center_axis',(0.866185586048601,0.432774614486463,-0.249857286421141));
#20759=DIRECTION('ref_axis',(0.446950695480888,-0.89455859271998,1.05171903626344E-18));
#20760=DIRECTION('center_axis',(-3.0024060161137E-16,0.499992114975783,
0.866029956157432));
#20761=DIRECTION('ref_axis',(1.13450604310479E-33,-0.866029956157432,0.499992114975783));
#20762=DIRECTION('',(0.499722453489577,-0.750142665109869,0.433085963129978));
#20763=DIRECTION('',(-0.866185586048601,-0.432774614486463,0.249857286421141));
#20764=DIRECTION('',(0.499722453489577,-0.750142665109869,0.433085963129978));
#20765=DIRECTION('',(-0.866185586048601,-0.432774614486463,0.249857286421141));
#20766=DIRECTION('center_axis',(-0.499722453489577,0.750142665109869,-0.433085963129978));
#20767=DIRECTION('ref_axis',(0.832241064261676,0.554413934670291,-3.58035061299401E-18));
#20768=DIRECTION('',(0.,0.499992114975783,0.866029956157432));
#20769=DIRECTION('',(0.,0.499992114975783,0.866029956157432));
#20770=DIRECTION('',(-0.866185586048601,-0.432774614486463,0.249857286421141));
#20771=DIRECTION('center_axis',(0.,-0.499992114975783,-0.866029956157432));
#20772=DIRECTION('ref_axis',(0.,0.866029956157432,-0.499992114975783));
#20773=DIRECTION('',(-0.499722453489577,0.750142665109869,-0.433085963129978));
#20774=DIRECTION('',(-0.499722453489577,0.750142665109869,-0.433085963129978));
#20775=DIRECTION('',(-0.866185586048601,-0.432774614486463,0.249857286421141));
#20776=DIRECTION('center_axis',(0.499722453489577,-0.750142665109869,0.433085963129978));
#20777=DIRECTION('ref_axis',(-0.832241064261676,-0.554413934670291,3.58035061299401E-18));
#20778=DIRECTION('',(0.,-0.499992114975783,-0.866029956157432));
#20779=DIRECTION('',(0.,-0.499992114975783,-0.866029956157432));
#20780=DIRECTION('center_axis',(0.866185586048601,0.432774614486463,-0.249857286421141));
#20781=DIRECTION('ref_axis',(0.446950695480888,-0.89455859271998,1.05171903626344E-18));
#20782=DIRECTION('center_axis',(0.866185586048601,0.432774614486463,-0.249857286421141));
#20783=DIRECTION('ref_axis',(0.446950695480888,-0.89455859271998,1.05171903626344E-18));
#20784=DIRECTION('center_axis',(-3.0024060161137E-16,0.499992114975783,
0.866029956157432));
#20785=DIRECTION('ref_axis',(1.13450604310479E-33,-0.866029956157432,0.499992114975783));
#20786=DIRECTION('',(0.499722453489577,-0.750142665109869,0.433085963129978));
#20787=DIRECTION('',(-0.866185586048601,-0.432774614486463,0.249857286421141));
#20788=DIRECTION('',(0.499722453489577,-0.750142665109869,0.433085963129978));
#20789=DIRECTION('',(-0.866185586048601,-0.432774614486463,0.249857286421141));
#20790=DIRECTION('center_axis',(-0.499722453489577,0.750142665109869,-0.433085963129978));
#20791=DIRECTION('ref_axis',(0.832241064261676,0.554413934670291,-3.58035061299401E-18));
#20792=DIRECTION('',(0.,0.499992114975783,0.866029956157432));
#20793=DIRECTION('',(0.,0.499992114975783,0.866029956157432));
#20794=DIRECTION('',(-0.866185586048601,-0.432774614486463,0.249857286421141));
#20795=DIRECTION('center_axis',(0.,-0.499992114975783,-0.866029956157432));
#20796=DIRECTION('ref_axis',(0.,0.866029956157432,-0.499992114975783));
#20797=DIRECTION('',(-0.499722453489577,0.750142665109869,-0.433085963129978));
#20798=DIRECTION('',(-0.499722453489577,0.750142665109869,-0.433085963129978));
#20799=DIRECTION('',(-0.866185586048601,-0.432774614486463,0.249857286421141));
#20800=DIRECTION('center_axis',(0.499722453489577,-0.750142665109869,0.433085963129978));
#20801=DIRECTION('ref_axis',(-0.832241064261676,-0.554413934670291,3.58035061299401E-18));
#20802=DIRECTION('',(0.,-0.499992114975783,-0.866029956157432));
#20803=DIRECTION('',(0.,-0.499992114975783,-0.866029956157432));
#20804=DIRECTION('center_axis',(0.866185586048601,0.432774614486463,-0.249857286421141));
#20805=DIRECTION('ref_axis',(0.446950695480888,-0.89455859271998,1.05171903626344E-18));
#20806=DIRECTION('center_axis',(0.866185586048601,0.432774614486463,-0.249857286421141));
#20807=DIRECTION('ref_axis',(0.446950695480888,-0.89455859271998,1.05171903626344E-18));
#20808=DIRECTION('center_axis',(7.72189864380049E-11,-0.866021775524098,
0.500006284278597));
#20809=DIRECTION('ref_axis',(9.43920741915831E-6,0.500006284256323,0.866021775485517));
#20810=DIRECTION('',(-0.999999999955451,4.71959615486962E-6,8.17459777866693E-6));
#20811=DIRECTION('',(9.43920741915831E-6,0.500006284256323,0.866021775485517));
#20812=DIRECTION('',(-0.999999999955451,4.71959615486962E-6,8.17459777866693E-6));
#20813=DIRECTION('',(9.43920741915831E-6,0.500006284256323,0.866021775485517));
#20814=DIRECTION('center_axis',(0.866185585971425,0.43276643839414,-0.249871447858675));
#20815=DIRECTION('ref_axis',(-0.44695491741627,0.447282837726406,-0.774705986082997));
#20816=DIRECTION('',(0.4997224535342,-0.75013793765136,0.433094151345782));
#20817=DIRECTION('',(0.4997224535342,-0.75013793765136,0.433094151345782));
#20818=DIRECTION('',(9.43920741915831E-6,0.500006284256323,0.866021775485517));
#20819=DIRECTION('center_axis',(-7.72188184696774E-11,0.866021775524098,
-0.500006284278597));
#20820=DIRECTION('ref_axis',(-9.43920741915831E-6,-0.500006284256323,-0.866021775485517));
#20821=DIRECTION('',(0.999999999955451,-4.71959615501004E-6,-8.17459777857421E-6));
#20822=DIRECTION('',(0.999999999955451,-4.71959615501004E-6,-8.17459777857421E-6));
#20823=DIRECTION('',(9.43920741915831E-6,0.500006284256323,0.866021775485517));
#20824=DIRECTION('center_axis',(-0.866185586048601,0.432774614486463,-0.24985728642114));
#20825=DIRECTION('ref_axis',(-0.446946473505681,-0.447278618872838,0.774713293367322));
#20826=DIRECTION('',(0.499722453400429,0.75013322067502,-0.433102321405899));
#20827=DIRECTION('',(0.499722453400429,0.75013322067502,-0.433102321405899));
#20828=DIRECTION('center_axis',(-9.43920741916839E-6,-0.500006284256323,
-0.866021775485517));
#20829=DIRECTION('ref_axis',(7.72188184718094E-11,-0.866021775524098,0.500006284278598));
#20830=DIRECTION('center_axis',(-9.43920741916839E-6,-0.500006284256323,
-0.866021775485517));
#20831=DIRECTION('ref_axis',(7.72188184718094E-11,-0.866021775524098,0.500006284278598));
#20832=DIRECTION('center_axis',(-1.,1.68317620470764E-16,0.));
#20833=DIRECTION('ref_axis',(-1.68317620470764E-16,-1.,0.));
#20834=DIRECTION('',(-1.68317620470764E-16,-1.,0.));
#20835=DIRECTION('',(0.,0.,1.));
#20836=DIRECTION('',(-1.68317620470764E-16,-1.,0.));
#20837=DIRECTION('',(0.,0.,1.));
#20838=DIRECTION('center_axis',(0.,1.,0.));
#20839=DIRECTION('ref_axis',(0.,0.,1.));
#20840=DIRECTION('',(-1.,0.,0.));
#20841=DIRECTION('',(0.,0.,1.));
#20842=DIRECTION('',(-1.,0.,0.));
#20843=DIRECTION('center_axis',(1.,0.,0.));
#20844=DIRECTION('ref_axis',(0.,0.,-1.));
#20845=DIRECTION('',(0.,1.,0.));
#20846=DIRECTION('',(0.,0.,1.));
#20847=DIRECTION('',(0.,1.,0.));
#20848=DIRECTION('center_axis',(0.,-1.,0.));
#20849=DIRECTION('ref_axis',(0.,0.,-1.));
#20850=DIRECTION('',(1.,0.,0.));
#20851=DIRECTION('',(1.,0.,0.));
#20852=DIRECTION('center_axis',(0.,0.,-1.));
#20853=DIRECTION('ref_axis',(-1.,0.,0.));
#20854=DIRECTION('center_axis',(0.,0.,-1.));
#20855=DIRECTION('ref_axis',(-1.,0.,0.));
#20856=DIRECTION('center_axis',(-1.,1.68317620470764E-16,0.));
#20857=DIRECTION('ref_axis',(-1.68317620470764E-16,-1.,0.));
#20858=DIRECTION('',(-1.68317620470764E-16,-1.,0.));
#20859=DIRECTION('',(0.,0.,1.));
#20860=DIRECTION('',(-1.68317620470764E-16,-1.,0.));
#20861=DIRECTION('',(0.,0.,1.));
#20862=DIRECTION('center_axis',(0.,1.,0.));
#20863=DIRECTION('ref_axis',(0.,0.,1.));
#20864=DIRECTION('',(-1.,0.,0.));
#20865=DIRECTION('',(0.,0.,1.));
#20866=DIRECTION('',(-1.,0.,0.));
#20867=DIRECTION('center_axis',(1.,-1.68317620470764E-16,0.));
#20868=DIRECTION('ref_axis',(1.68317620470764E-16,1.,0.));
#20869=DIRECTION('',(1.68317620470764E-16,1.,0.));
#20870=DIRECTION('',(0.,0.,1.));
#20871=DIRECTION('',(1.68317620470764E-16,1.,0.));
#20872=DIRECTION('center_axis',(0.,-1.,0.));
#20873=DIRECTION('ref_axis',(0.,0.,-1.));
#20874=DIRECTION('',(1.,0.,0.));
#20875=DIRECTION('',(1.,0.,0.));
#20876=DIRECTION('center_axis',(0.,0.,-1.));
#20877=DIRECTION('ref_axis',(-1.,0.,0.));
#20878=DIRECTION('center_axis',(0.,0.,-1.));
#20879=DIRECTION('ref_axis',(-1.,0.,0.));
#20880=DIRECTION('center_axis',(-1.,0.,0.));
#20881=DIRECTION('ref_axis',(0.,0.,1.));
#20882=DIRECTION('',(0.,-1.,0.));
#20883=DIRECTION('',(0.,0.,1.));
#20884=DIRECTION('',(0.,-1.,0.));
#20885=DIRECTION('',(0.,0.,1.));
#20886=DIRECTION('center_axis',(0.,1.,0.));
#20887=DIRECTION('ref_axis',(0.,0.,1.));
#20888=DIRECTION('',(-1.,0.,0.));
#20889=DIRECTION('',(0.,0.,1.));
#20890=DIRECTION('',(-1.,0.,0.));
#20891=DIRECTION('center_axis',(1.,0.,0.));
#20892=DIRECTION('ref_axis',(0.,0.,-1.));
#20893=DIRECTION('',(0.,1.,0.));
#20894=DIRECTION('',(0.,0.,1.));
#20895=DIRECTION('',(0.,1.,0.));
#20896=DIRECTION('center_axis',(0.,-1.,0.));
#20897=DIRECTION('ref_axis',(0.,0.,-1.));
#20898=DIRECTION('',(1.,0.,0.));
#20899=DIRECTION('',(1.,0.,0.));
#20900=DIRECTION('center_axis',(0.,0.,1.));
#20901=DIRECTION('ref_axis',(1.,0.,0.));
#20902=DIRECTION('center_axis',(0.,0.,1.));
#20903=DIRECTION('ref_axis',(1.,0.,0.));
#20904=DIRECTION('center_axis',(-1.,0.,0.));
#20905=DIRECTION('ref_axis',(0.,0.,1.));
#20906=DIRECTION('',(0.,-1.,0.));
#20907=DIRECTION('',(0.,0.,1.));
#20908=DIRECTION('',(0.,-1.,0.));
#20909=DIRECTION('',(0.,0.,1.));
#20910=DIRECTION('center_axis',(0.,1.,0.));
#20911=DIRECTION('ref_axis',(0.,0.,1.));
#20912=DIRECTION('',(-1.,0.,0.));
#20913=DIRECTION('',(0.,0.,1.));
#20914=DIRECTION('',(-1.,0.,0.));
#20915=DIRECTION('center_axis',(1.,0.,0.));
#20916=DIRECTION('ref_axis',(0.,0.,-1.));
#20917=DIRECTION('',(0.,1.,0.));
#20918=DIRECTION('',(0.,0.,1.));
#20919=DIRECTION('',(0.,1.,0.));
#20920=DIRECTION('center_axis',(0.,-1.,0.));
#20921=DIRECTION('ref_axis',(0.,0.,-1.));
#20922=DIRECTION('',(1.,0.,0.));
#20923=DIRECTION('',(1.,0.,0.));
#20924=DIRECTION('center_axis',(0.,0.,1.));
#20925=DIRECTION('ref_axis',(1.,0.,0.));
#20926=DIRECTION('center_axis',(0.,0.,1.));
#20927=DIRECTION('ref_axis',(1.,0.,0.));
#20928=DIRECTION('center_axis',(-1.,3.73454720419507E-16,0.));
#20929=DIRECTION('ref_axis',(-3.73454720419507E-16,-1.,0.));
#20930=DIRECTION('',(-3.73454720419507E-16,-1.,0.));
#20931=DIRECTION('',(0.,0.,1.));
#20932=DIRECTION('',(-3.73454720419507E-16,-1.,0.));
#20933=DIRECTION('',(0.,0.,1.));
#20934=DIRECTION('center_axis',(0.,1.,0.));
#20935=DIRECTION('ref_axis',(0.,0.,1.));
#20936=DIRECTION('',(-1.,0.,0.));
#20937=DIRECTION('',(0.,0.,1.));
#20938=DIRECTION('',(-1.,0.,0.));
#20939=DIRECTION('center_axis',(1.,-3.36635240941527E-16,0.));
#20940=DIRECTION('ref_axis',(3.36635240941527E-16,1.,0.));
#20941=DIRECTION('',(3.36635240941527E-16,1.,0.));
#20942=DIRECTION('',(0.,0.,1.));
#20943=DIRECTION('',(3.36635240941527E-16,1.,0.));
#20944=DIRECTION('center_axis',(0.,-1.,0.));
#20945=DIRECTION('ref_axis',(0.,0.,-1.));
#20946=DIRECTION('',(1.,0.,0.));
#20947=DIRECTION('',(1.,0.,0.));
#20948=DIRECTION('center_axis',(0.,0.,-1.));
#20949=DIRECTION('ref_axis',(-1.,0.,0.));
#20950=DIRECTION('center_axis',(0.,0.,-1.));
#20951=DIRECTION('ref_axis',(-1.,0.,0.));
#20952=DIRECTION('center_axis',(-1.,6.73270481883054E-16,0.));
#20953=DIRECTION('ref_axis',(-6.73270481883054E-16,-1.,0.));
#20954=DIRECTION('',(-6.73270481883054E-16,-1.,0.));
#20955=DIRECTION('',(0.,0.,1.));
#20956=DIRECTION('',(-6.73270481883054E-16,-1.,0.));
#20957=DIRECTION('',(0.,0.,1.));
#20958=DIRECTION('center_axis',(0.,1.,0.));
#20959=DIRECTION('ref_axis',(0.,0.,1.));
#20960=DIRECTION('',(-1.,0.,0.));
#20961=DIRECTION('',(0.,0.,1.));
#20962=DIRECTION('',(-1.,0.,0.));
#20963=DIRECTION('center_axis',(1.,-6.73270481883054E-16,0.));
#20964=DIRECTION('ref_axis',(6.73270481883054E-16,1.,0.));
#20965=DIRECTION('',(6.73270481883054E-16,1.,0.));
#20966=DIRECTION('',(0.,0.,1.));
#20967=DIRECTION('',(6.73270481883054E-16,1.,0.));
#20968=DIRECTION('center_axis',(0.,-1.,0.));
#20969=DIRECTION('ref_axis',(0.,0.,-1.));
#20970=DIRECTION('',(1.,0.,0.));
#20971=DIRECTION('',(1.,0.,0.));
#20972=DIRECTION('center_axis',(0.,0.,-1.));
#20973=DIRECTION('ref_axis',(-1.,0.,0.));
#20974=DIRECTION('center_axis',(0.,0.,-1.));
#20975=DIRECTION('ref_axis',(-1.,0.,0.));
#20976=DIRECTION('axis',(0.,0.,1.));
#20977=DIRECTION('refdir',(1.,0.,0.));
#20978=DIRECTION('center_axis',(1.,0.,0.));
#20979=DIRECTION('ref_axis',(0.,0.,-1.));
#20980=DIRECTION('center_axis',(1.,0.,0.));
#20981=DIRECTION('ref_axis',(0.,0.,-1.));
#20982=DIRECTION('center_axis',(1.,0.,0.));
#20983=DIRECTION('ref_axis',(0.,0.,-1.));
#20984=DIRECTION('center_axis',(0.,1.,1.22464679914735E-16));
#20985=DIRECTION('ref_axis',(0.,-1.22464679914735E-16,1.));
#20986=DIRECTION('center_axis',(-1.,0.,0.));
#20987=DIRECTION('ref_axis',(0.,0.,-1.));
#20988=DIRECTION('center_axis',(-1.,0.,0.));
#20989=DIRECTION('ref_axis',(0.,0.,1.));
#20990=DIRECTION('center_axis',(-1.,0.,0.));
#20991=DIRECTION('ref_axis',(0.,0.,1.));
#20992=DIRECTION('center_axis',(-1.,0.,0.));
#20993=DIRECTION('ref_axis',(0.,0.,1.));
#20994=DIRECTION('center_axis',(-1.,0.,0.));
#20995=DIRECTION('ref_axis',(0.,0.,1.));
#20996=DIRECTION('',(1.,0.,0.));
#20997=DIRECTION('center_axis',(1.,0.,0.));
#20998=DIRECTION('ref_axis',(0.,0.,-1.));
#20999=DIRECTION('center_axis',(-1.,0.,0.));
#21000=DIRECTION('ref_axis',(0.,0.,1.));
#21001=DIRECTION('center_axis',(-1.,0.,0.));
#21002=DIRECTION('ref_axis',(0.,0.,1.));
#21003=DIRECTION('center_axis',(-1.,0.,0.));
#21004=DIRECTION('ref_axis',(0.,0.,1.));
#21005=DIRECTION('center_axis',(-1.,0.,0.));
#21006=DIRECTION('ref_axis',(0.,0.,1.));
#21007=DIRECTION('center_axis',(-1.,0.,0.));
#21008=DIRECTION('ref_axis',(0.,0.,1.));
#21009=DIRECTION('',(0.707106781186549,8.65956056235491E-17,0.707106781186546));
#21010=DIRECTION('center_axis',(-1.,0.,0.));
#21011=DIRECTION('ref_axis',(0.,0.,1.));
#21012=DIRECTION('center_axis',(-1.,0.,0.));
#21013=DIRECTION('ref_axis',(0.,0.,1.));
#21014=DIRECTION('',(1.,0.,0.));
#21015=DIRECTION('center_axis',(1.,0.,0.));
#21016=DIRECTION('ref_axis',(0.,0.,-1.));
#21017=DIRECTION('center_axis',(-1.,0.,0.));
#21018=DIRECTION('ref_axis',(0.,0.,1.));
#21019=DIRECTION('center_axis',(1.,0.,0.));
#21020=DIRECTION('ref_axis',(0.,0.,-1.));
#21021=DIRECTION('',(0.,0.500000000000001,0.866025403784438));
#21022=DIRECTION('',(0.,1.,2.22565125738838E-16));
#21023=DIRECTION('center_axis',(1.,0.,0.));
#21024=DIRECTION('ref_axis',(0.,0.,-1.));
#21025=DIRECTION('',(0.,0.500000000000001,0.866025403784438));
#21026=DIRECTION('',(0.,-0.500000000000001,0.866025403784438));
#21027=DIRECTION('center_axis',(1.,0.,0.));
#21028=DIRECTION('ref_axis',(0.,0.,-1.));
#21029=DIRECTION('',(0.,-0.500000000000001,0.866025403784438));
#21030=DIRECTION('',(0.,-1.,2.22565125738839E-16));
#21031=DIRECTION('center_axis',(1.,0.,0.));
#21032=DIRECTION('ref_axis',(0.,0.,-1.));
#21033=DIRECTION('',(0.,-1.,2.22565125738839E-16));
#21034=DIRECTION('',(0.,-0.500000000000001,-0.866025403784438));
#21035=DIRECTION('center_axis',(1.,0.,0.));
#21036=DIRECTION('ref_axis',(0.,0.,-1.));
#21037=DIRECTION('',(0.,-0.500000000000001,-0.866025403784438));
#21038=DIRECTION('',(0.,0.5,-0.866025403784439));
#21039=DIRECTION('center_axis',(1.,0.,0.));
#21040=DIRECTION('ref_axis',(0.,0.,-1.));
#21041=DIRECTION('',(0.,0.5,-0.866025403784439));
#21042=DIRECTION('',(0.,1.,2.22565125738838E-16));
#21043=DIRECTION('center_axis',(1.,0.,0.));
#21044=DIRECTION('ref_axis',(0.,0.,-1.));
#21045=DIRECTION('center_axis',(1.,0.,0.));
#21046=DIRECTION('ref_axis',(0.,0.,-1.));
#21047=DIRECTION('center_axis',(1.,0.,0.));
#21048=DIRECTION('ref_axis',(0.,0.,-1.));
#21049=DIRECTION('center_axis',(1.,0.,0.));
#21050=DIRECTION('ref_axis',(0.,0.,-1.));
#21051=DIRECTION('center_axis',(1.,0.,0.));
#21052=DIRECTION('ref_axis',(0.,0.,-1.));
#21053=DIRECTION('center_axis',(-1.,0.,0.));
#21054=DIRECTION('ref_axis',(0.,0.,1.));
#21055=DIRECTION('center_axis',(1.,0.,0.));
#21056=DIRECTION('ref_axis',(0.,0.,-1.));
#21057=DIRECTION('center_axis',(1.,0.,0.));
#21058=DIRECTION('ref_axis',(0.,0.,-1.));
#21059=DIRECTION('center_axis',(1.,0.,0.));
#21060=DIRECTION('ref_axis',(0.,0.,-1.));
#21061=DIRECTION('center_axis',(1.,0.,0.));
#21062=DIRECTION('ref_axis',(0.,0.,-1.));
#21063=DIRECTION('center_axis',(1.,0.,0.));
#21064=DIRECTION('ref_axis',(0.,0.,-1.));
#21065=DIRECTION('center_axis',(1.,0.,0.));
#21066=DIRECTION('ref_axis',(0.,0.,-1.));
#21067=DIRECTION('center_axis',(1.,0.,0.));
#21068=DIRECTION('ref_axis',(0.,0.,-1.));
#21069=DIRECTION('center_axis',(0.,-2.22565125738838E-16,1.));
#21070=DIRECTION('ref_axis',(0.,-1.,-2.22565125738838E-16));
#21071=DIRECTION('',(-1.,0.,0.));
#21072=DIRECTION('',(-1.,0.,0.));
#21073=DIRECTION('center_axis',(0.,0.866025403784439,0.5));
#21074=DIRECTION('ref_axis',(0.,-0.5,0.866025403784439));
#21075=DIRECTION('',(-1.,0.,0.));
#21076=DIRECTION('center_axis',(0.,0.866025403784438,-0.500000000000001));
#21077=DIRECTION('ref_axis',(0.,0.500000000000001,0.866025403784438));
#21078=DIRECTION('',(-1.,0.,0.));
#21079=DIRECTION('center_axis',(0.,-2.22565125738839E-16,-1.));
#21080=DIRECTION('ref_axis',(0.,1.,-2.22565125738839E-16));
#21081=DIRECTION('',(-1.,0.,0.));
#21082=DIRECTION('center_axis',(0.,-0.866025403784438,-0.500000000000001));
#21083=DIRECTION('ref_axis',(0.,0.500000000000001,-0.866025403784438));
#21084=DIRECTION('',(-1.,0.,0.));
#21085=DIRECTION('center_axis',(0.,-0.866025403784438,0.500000000000001));
#21086=DIRECTION('ref_axis',(0.,-0.500000000000001,-0.866025403784438));
#21087=DIRECTION('axis',(0.,0.,1.));
#21088=DIRECTION('refdir',(1.,0.,0.));
#21089=DIRECTION('center_axis',(-1.,0.,0.));
#21090=DIRECTION('ref_axis',(0.,0.,1.));
#21091=DIRECTION('center_axis',(-1.,0.,0.));
#21092=DIRECTION('ref_axis',(0.,0.,1.));
#21093=DIRECTION('',(1.,0.,0.));
#21094=DIRECTION('center_axis',(-1.,0.,0.));
#21095=DIRECTION('ref_axis',(0.,0.,1.));
#21096=DIRECTION('center_axis',(-1.,0.,0.));
#21097=DIRECTION('ref_axis',(0.,0.,1.));
#21098=DIRECTION('center_axis',(-1.,0.,0.));
#21099=DIRECTION('ref_axis',(0.,0.,1.));
#21100=DIRECTION('',(-1.,0.,0.));
#21101=DIRECTION('center_axis',(-1.,0.,0.));
#21102=DIRECTION('ref_axis',(0.,0.,1.));
#21103=DIRECTION('center_axis',(-1.,0.,0.));
#21104=DIRECTION('ref_axis',(0.,0.,1.));
#21105=DIRECTION('center_axis',(1.,0.,0.));
#21106=DIRECTION('ref_axis',(0.,0.,-1.));
#21107=DIRECTION('axis',(0.,0.,1.));
#21108=DIRECTION('refdir',(1.,0.,0.));
#21109=DIRECTION('center_axis',(0.,0.,1.));
#21110=DIRECTION('ref_axis',(1.,0.,0.));
#21111=DIRECTION('center_axis',(0.,0.,1.));
#21112=DIRECTION('ref_axis',(-1.,0.,0.));
#21113=DIRECTION('',(0.,0.,1.));
#21114=DIRECTION('center_axis',(0.,0.,1.));
#21115=DIRECTION('ref_axis',(1.,0.,0.));
#21116=DIRECTION('center_axis',(0.,0.,1.));
#21117=DIRECTION('ref_axis',(1.,0.,0.));
#21118=DIRECTION('center_axis',(0.,0.,-1.));
#21119=DIRECTION('ref_axis',(-1.,0.,0.));
#21120=DIRECTION('center_axis',(0.,0.,1.));
#21121=DIRECTION('ref_axis',(-1.,0.,0.));
#21122=DIRECTION('',(0.819152044288991,-1.00317192905352E-16,-0.573576436351047));
#21123=DIRECTION('center_axis',(0.,0.,1.));
#21124=DIRECTION('ref_axis',(-1.,0.,0.));
#21125=DIRECTION('center_axis',(0.,0.,1.));
#21126=DIRECTION('ref_axis',(1.,0.,0.));
#21127=DIRECTION('center_axis',(0.,0.,-1.));
#21128=DIRECTION('ref_axis',(1.,0.,0.));
#21129=DIRECTION('',(-0.819152044288991,-1.00317192905352E-16,0.573576436351047));
#21130=DIRECTION('center_axis',(0.,0.,1.));
#21131=DIRECTION('ref_axis',(1.,0.,0.));
#21132=DIRECTION('center_axis',(0.,0.,1.));
#21133=DIRECTION('ref_axis',(1.,0.,0.));
#21134=DIRECTION('',(0.,0.,1.));
#21135=DIRECTION('center_axis',(-0.500000000000001,0.866025403784438,0.));
#21136=DIRECTION('ref_axis',(-0.866025403784438,-0.500000000000001,0.));
#21137=DIRECTION('',(0.,0.,1.));
#21138=DIRECTION('',(0.,0.,1.));
#21139=DIRECTION('center_axis',(0.500000000000001,0.866025403784438,0.));
#21140=DIRECTION('ref_axis',(-0.866025403784438,0.500000000000001,0.));
#21141=DIRECTION('',(0.,0.,1.));
#21142=DIRECTION('center_axis',(-1.,0.,0.));
#21143=DIRECTION('ref_axis',(0.,0.,1.));
#21144=DIRECTION('',(0.,0.,1.));
#21145=DIRECTION('center_axis',(0.500000000000001,-0.866025403784438,0.));
#21146=DIRECTION('ref_axis',(0.866025403784438,0.500000000000001,0.));
#21147=DIRECTION('',(0.,0.,1.));
#21148=DIRECTION('center_axis',(-0.500000000000001,-0.866025403784438,0.));
#21149=DIRECTION('ref_axis',(0.866025403784438,-0.500000000000001,0.));
#21150=DIRECTION('',(0.,0.,1.));
#21151=DIRECTION('center_axis',(-1.,0.,0.));
#21152=DIRECTION('ref_axis',(0.,0.,1.));
#21153=DIRECTION('center_axis',(0.,0.,-1.));
#21154=DIRECTION('ref_axis',(-1.,0.,0.));
#21155=DIRECTION('center_axis',(0.,0.,-1.));
#21156=DIRECTION('ref_axis',(-1.,0.,0.));
#21157=DIRECTION('center_axis',(0.,0.,-1.));
#21158=DIRECTION('ref_axis',(-1.,0.,0.));
#21159=DIRECTION('center_axis',(0.,0.,-1.));
#21160=DIRECTION('ref_axis',(-1.,0.,0.));
#21161=DIRECTION('center_axis',(0.,0.,-1.));
#21162=DIRECTION('ref_axis',(-1.,0.,0.));
#21163=DIRECTION('center_axis',(0.,0.,1.));
#21164=DIRECTION('ref_axis',(1.,0.,0.));
#21165=DIRECTION('center_axis',(0.,0.,-1.));
#21166=DIRECTION('ref_axis',(-1.,0.,0.));
#21167=DIRECTION('center_axis',(0.,0.,-1.));
#21168=DIRECTION('ref_axis',(-1.,0.,0.));
#21169=DIRECTION('center_axis',(0.,0.,1.));
#21170=DIRECTION('ref_axis',(-1.,0.,0.));
#21171=DIRECTION('center_axis',(0.,0.,1.));
#21172=DIRECTION('ref_axis',(-1.,-8.88178419700125E-16,0.));
#21173=DIRECTION('center_axis',(0.,0.,1.));
#21174=DIRECTION('ref_axis',(-1.,3.5527136788005E-15,0.));
#21175=DIRECTION('center_axis',(0.,0.,1.));
#21176=DIRECTION('ref_axis',(1.,0.,0.));
#21177=DIRECTION('center_axis',(0.,0.,1.));
#21178=DIRECTION('ref_axis',(-1.,1.77635683940025E-15,0.));
#21179=DIRECTION('center_axis',(0.,0.,1.));
#21180=DIRECTION('ref_axis',(-1.,0.,0.));
#21181=DIRECTION('center_axis',(0.,0.,1.));
#21182=DIRECTION('ref_axis',(1.,0.,0.));
#21183=DIRECTION('center_axis',(0.,0.,1.));
#21184=DIRECTION('ref_axis',(1.,0.,0.));
#21185=DIRECTION('center_axis',(0.,0.,1.));
#21186=DIRECTION('ref_axis',(1.,0.,0.));
#21187=DIRECTION('center_axis',(0.,0.,1.));
#21188=DIRECTION('ref_axis',(1.,0.,0.));
#21189=DIRECTION('center_axis',(0.,0.,1.));
#21190=DIRECTION('ref_axis',(1.,0.,0.));
#21191=DIRECTION('center_axis',(0.,0.,1.));
#21192=DIRECTION('ref_axis',(1.,0.,0.));
#21193=DIRECTION('center_axis',(0.,0.,-1.));
#21194=DIRECTION('ref_axis',(-1.,0.,0.));
#21195=DIRECTION('center_axis',(0.,0.,-1.));
#21196=DIRECTION('ref_axis',(-1.,0.,0.));
#21197=DIRECTION('center_axis',(0.,0.,-1.));
#21198=DIRECTION('ref_axis',(-1.,0.,0.));
#21199=DIRECTION('center_axis',(0.,0.,-1.));
#21200=DIRECTION('ref_axis',(-1.,0.,0.));
#21201=DIRECTION('center_axis',(0.,0.,-1.));
#21202=DIRECTION('ref_axis',(-1.,0.,0.));
#21203=DIRECTION('center_axis',(0.,0.,-1.));
#21204=DIRECTION('ref_axis',(-1.,0.,0.));
#21205=DIRECTION('',(0.,0.,1.));
#21206=DIRECTION('',(1.,0.,0.));
#21207=DIRECTION('',(1.,-1.23908044646905E-32,-1.87133061054672E-16));
#21208=DIRECTION('',(-1.87133061054672E-16,-9.11574503592941E-64,-1.));
#21209=DIRECTION('',(-2.64697796016969E-23,-1.,2.88998133608509E-16));
#21210=DIRECTION('',(1.,-2.64697796016969E-23,-2.64697796016969E-23));
#21211=DIRECTION('',(0.,0.,1.));
#21212=DIRECTION('',(1.,0.,0.));
#21213=DIRECTION('',(1.,1.11022302462516E-16,0.));
#21214=DIRECTION('',(1.11022302462516E-16,-1.,1.23259516440783E-32));
#21215=DIRECTION('',(1.,0.,0.));
#21216=DIRECTION('',(0.,1.,0.));
#21217=DIRECTION('',(0.,-1.,0.));
#21218=DIRECTION('',(1.,0.,0.));
#21219=DIRECTION('',(1.,1.11022302462516E-16,0.));
#21220=DIRECTION('',(1.11022302462516E-16,-1.,1.23259516440783E-32));
#21221=DIRECTION('',(1.,1.11022302462516E-16,0.));
#21222=DIRECTION('',(1.11022302462516E-16,-1.,1.23259516440783E-32));
#21223=DIRECTION('',(1.,1.11022302462516E-16,0.));
#21224=DIRECTION('',(1.11022302462516E-16,-1.,1.23259516440783E-32));
#21225=DIRECTION('',(1.,1.11022302462516E-16,0.));
#21226=DIRECTION('',(1.11022302462516E-16,-1.,1.23259516440783E-32));
#21227=DIRECTION('',(1.,1.11022302462516E-16,0.));
#21228=DIRECTION('',(1.11022302462516E-16,-1.,1.23259516440783E-32));
#21229=DIRECTION('',(1.,1.11022302462516E-16,0.));
#21230=DIRECTION('',(1.11022302462516E-16,-1.,1.23259516440783E-32));
#21231=DIRECTION('',(1.,1.11022302462516E-16,0.));
#21232=DIRECTION('',(1.11022302462516E-16,-1.,1.23259516440783E-32));
#21233=DIRECTION('',(1.,1.11022302462516E-16,0.));
#21234=DIRECTION('',(1.11022302462516E-16,-1.,1.23259516440783E-32));
#21235=DIRECTION('',(1.,1.11022302462516E-16,0.));
#21236=DIRECTION('',(1.11022302462516E-16,-1.,1.23259516440783E-32));
#21237=DIRECTION('',(1.,1.11022302462516E-16,0.));
#21238=DIRECTION('',(1.11022302462516E-16,-1.,1.23259516440783E-32));
#21239=DIRECTION('',(1.,1.11022302462516E-16,0.));
#21240=DIRECTION('',(1.11022302462516E-16,-1.,1.23259516440783E-32));
#21241=DIRECTION('',(1.,1.11022302462516E-16,0.));
#21242=DIRECTION('',(1.11022302462516E-16,-1.,1.23259516440783E-32));
#21243=DIRECTION('',(1.,1.11022302462516E-16,0.));
#21244=DIRECTION('',(1.11022302462516E-16,-1.,1.23259516440783E-32));
#21245=DIRECTION('',(1.,1.11022302462516E-16,0.));
#21246=DIRECTION('',(1.11022302462516E-16,-1.,1.23259516440783E-32));
#21247=DIRECTION('',(1.,1.11022302462516E-16,0.));
#21248=DIRECTION('',(1.11022302462516E-16,-1.,1.23259516440783E-32));
#21249=DIRECTION('',(1.,0.,0.));
#21250=DIRECTION('',(0.,1.,0.));
#21251=DIRECTION('',(1.,0.,0.));
#21252=DIRECTION('',(0.,1.,0.));
#21253=DIRECTION('',(1.,0.,0.));
#21254=DIRECTION('',(0.,1.,0.));
#21255=DIRECTION('',(1.,0.,0.));
#21256=DIRECTION('',(0.,1.,0.));
#21257=DIRECTION('',(1.,0.,0.));
#21258=DIRECTION('',(0.,1.,0.));
#21259=DIRECTION('',(1.,0.,0.));
#21260=DIRECTION('',(0.,1.,0.));
#21261=DIRECTION('',(1.,0.,0.));
#21262=DIRECTION('',(0.,1.,0.));
#21263=DIRECTION('',(1.,0.,0.));
#21264=DIRECTION('',(0.,1.,0.));
#21265=DIRECTION('',(1.,0.,0.));
#21266=DIRECTION('',(0.,1.,0.));
#21267=DIRECTION('',(1.,0.,0.));
#21268=DIRECTION('',(0.,1.,0.));
#21269=DIRECTION('',(1.,0.,0.));
#21270=DIRECTION('',(0.,1.,0.));
#21271=DIRECTION('',(1.,0.,0.));
#21272=DIRECTION('',(0.,1.,0.));
#21273=DIRECTION('',(1.,0.,0.));
#21274=DIRECTION('',(0.,1.,0.));
#21275=DIRECTION('',(1.,0.,0.));
#21276=DIRECTION('',(0.,1.,0.));
#21277=DIRECTION('',(1.,0.,0.));
#21278=DIRECTION('',(0.,1.,0.));
#21279=DIRECTION('',(0.,-1.,0.));
#21280=DIRECTION('',(1.,0.,0.));
#21281=DIRECTION('',(0.,-1.,0.));
#21282=DIRECTION('',(1.,0.,0.));
#21283=DIRECTION('',(0.,-1.,0.));
#21284=DIRECTION('',(1.,0.,0.));
#21285=DIRECTION('',(0.,-1.,0.));
#21286=DIRECTION('',(1.,0.,0.));
#21287=DIRECTION('',(0.,-1.,0.));
#21288=DIRECTION('',(1.,0.,0.));
#21289=DIRECTION('',(0.,-1.,0.));
#21290=DIRECTION('',(1.,0.,0.));
#21291=DIRECTION('',(0.,-1.,0.));
#21292=DIRECTION('',(1.,0.,0.));
#21293=DIRECTION('',(0.,-1.,0.));
#21294=DIRECTION('',(1.,0.,0.));
#21295=DIRECTION('',(0.,-1.,0.));
#21296=DIRECTION('',(1.,0.,0.));
#21297=DIRECTION('',(0.,-1.,0.));
#21298=DIRECTION('',(1.,0.,0.));
#21299=DIRECTION('',(0.,-1.,0.));
#21300=DIRECTION('',(1.,0.,0.));
#21301=DIRECTION('',(0.,-1.,0.));
#21302=DIRECTION('',(1.,0.,0.));
#21303=DIRECTION('',(0.,-1.,0.));
#21304=DIRECTION('',(1.,0.,0.));
#21305=DIRECTION('',(0.,-1.,0.));
#21306=DIRECTION('',(1.,0.,0.));
#21307=DIRECTION('',(0.,-1.,0.));
#21308=DIRECTION('',(1.,0.,0.));
#21309=CARTESIAN_POINT('',(0.,0.,0.));
#21310=CARTESIAN_POINT('',(0.,0.,0.));
#21311=CARTESIAN_POINT('Origin',(400.,-261.,-12.7));
#21312=CARTESIAN_POINT('',(400.,-261.,0.));
#21313=CARTESIAN_POINT('',(400.,261.,0.));
#21314=CARTESIAN_POINT('',(400.,-261.,0.));
#21315=CARTESIAN_POINT('',(400.,-261.,-12.7));
#21316=CARTESIAN_POINT('',(400.,-261.,-12.7));
#21317=CARTESIAN_POINT('',(400.,261.,-12.7));
#21318=CARTESIAN_POINT('',(400.,-261.,-12.7));
#21319=CARTESIAN_POINT('',(400.,261.,-12.7));
#21320=CARTESIAN_POINT('Origin',(-400.,-261.,-12.7));
#21321=CARTESIAN_POINT('',(-400.,-261.,0.));
#21322=CARTESIAN_POINT('',(-400.,-261.,0.));
#21323=CARTESIAN_POINT('',(-400.,-261.,-12.7));
#21324=CARTESIAN_POINT('',(-400.,-261.,-12.7));
#21325=CARTESIAN_POINT('',(-400.,-261.,-12.7));
#21326=CARTESIAN_POINT('Origin',(-400.,-261.,-12.7));
#21327=CARTESIAN_POINT('',(-400.,261.,0.));
#21328=CARTESIAN_POINT('',(-400.,-261.,0.));
#21329=CARTESIAN_POINT('',(-400.,261.,-12.7));
#21330=CARTESIAN_POINT('',(-400.,261.,-12.7));
#21331=CARTESIAN_POINT('',(-400.,-261.,-12.7));
#21332=CARTESIAN_POINT('Origin',(-400.,261.,-12.7));
#21333=CARTESIAN_POINT('',(-400.,261.,0.));
#21334=CARTESIAN_POINT('',(-400.,261.,-12.7));
#21335=CARTESIAN_POINT('Origin',(0.,0.,-12.7));
#21336=CARTESIAN_POINT('',(250.,-200.,-12.7));
#21337=CARTESIAN_POINT('',(250.,200.,-12.7));
#21338=CARTESIAN_POINT('',(250.,-200.,-12.7));
#21339=CARTESIAN_POINT('',(-250.,200.,-12.7));
#21340=CARTESIAN_POINT('',(-250.,200.,-12.7));
#21341=CARTESIAN_POINT('',(-250.,-200.,-12.7));
#21342=CARTESIAN_POINT('',(-250.,-200.,-12.7));
#21343=CARTESIAN_POINT('',(-250.,-200.,-12.7));
#21344=CARTESIAN_POINT('Origin',(0.,0.,0.));
#21345=CARTESIAN_POINT('',(250.,200.,0.));
#21346=CARTESIAN_POINT('',(-250.,200.,0.));
#21347=CARTESIAN_POINT('',(-250.,200.,0.));
#21348=CARTESIAN_POINT('',(250.,-200.,0.));
#21349=CARTESIAN_POINT('',(250.,-200.,0.));
#21350=CARTESIAN_POINT('',(-250.,-200.,0.));
#21351=CARTESIAN_POINT('',(-250.,-200.,0.));
#21352=CARTESIAN_POINT('',(-250.,-200.,0.));
#21353=CARTESIAN_POINT('Origin',(250.,-200.,-12.7));
#21354=CARTESIAN_POINT('',(250.,200.,-12.7));
#21355=CARTESIAN_POINT('',(250.,-200.,-12.7));
#21356=CARTESIAN_POINT('Origin',(-250.,-200.,-12.7));
#21357=CARTESIAN_POINT('',(-250.,-200.,-12.7));
#21358=CARTESIAN_POINT('Origin',(-250.,-200.,-12.7));
#21359=CARTESIAN_POINT('',(-250.,200.,-12.7));
#21360=CARTESIAN_POINT('Origin',(-250.,200.,-12.7));
#21361=CARTESIAN_POINT('Origin',(412.7,261.,-12.7));
#21362=CARTESIAN_POINT('',(400.,261.,-12.7));
#21363=CARTESIAN_POINT('',(400.,-261.,-12.7));
#21364=CARTESIAN_POINT('',(400.,261.,-12.7));
#21365=CARTESIAN_POINT('',(412.7,-261.,-12.7));
#21366=CARTESIAN_POINT('',(412.7,-261.,-12.7));
#21367=CARTESIAN_POINT('',(412.7,261.,-12.7));
#21368=CARTESIAN_POINT('',(412.7,261.,-12.7));
#21369=CARTESIAN_POINT('',(412.7,261.,-12.7));
#21370=CARTESIAN_POINT('Origin',(412.7,-261.,-589.215307716505));
#21371=CARTESIAN_POINT('',(400.,-261.,-589.215307716505));
#21372=CARTESIAN_POINT('',(400.,-261.,-589.215307716505));
#21373=CARTESIAN_POINT('',(412.7,-261.,-589.215307716505));
#21374=CARTESIAN_POINT('',(412.7,-261.,-589.215307716505));
#21375=CARTESIAN_POINT('',(412.7,-261.,-589.215307716505));
#21376=CARTESIAN_POINT('Origin',(412.7,-276.,-662.7));
#21377=CARTESIAN_POINT('',(400.,-201.,-662.7));
#21378=CARTESIAN_POINT('Origin',(400.,-276.,-662.7));
#21379=CARTESIAN_POINT('',(412.7,-201.,-662.7));
#21380=CARTESIAN_POINT('',(412.7,-201.,-662.7));
#21381=CARTESIAN_POINT('Origin',(412.7,-276.,-662.7));
#21382=CARTESIAN_POINT('Origin',(412.7,-201.,-1012.7));
#21383=CARTESIAN_POINT('',(400.,-201.,-1012.7));
#21384=CARTESIAN_POINT('',(400.,-201.,-1012.7));
#21385=CARTESIAN_POINT('',(412.7,-201.,-1012.7));
#21386=CARTESIAN_POINT('',(412.7,-201.,-1012.7));
#21387=CARTESIAN_POINT('',(412.7,-201.,-1012.7));
#21388=CARTESIAN_POINT('Origin',(412.7,261.,-1012.7));
#21389=CARTESIAN_POINT('',(400.,261.,-1012.7));
#21390=CARTESIAN_POINT('',(400.,261.,-1012.7));
#21391=CARTESIAN_POINT('',(412.7,261.,-1012.7));
#21392=CARTESIAN_POINT('',(412.7,261.,-1012.7));
#21393=CARTESIAN_POINT('',(412.7,261.,-1012.7));
#21394=CARTESIAN_POINT('Origin',(412.7,261.,-12.7));
#21395=CARTESIAN_POINT('',(400.,261.,-12.7));
#21396=CARTESIAN_POINT('',(412.7,261.,-12.7));
#21397=CARTESIAN_POINT('Origin',(412.7,-276.,-662.7));
#21398=CARTESIAN_POINT('Origin',(400.,-276.,-662.7));
#21399=CARTESIAN_POINT('Origin',(-412.7,261.,-12.7));
#21400=CARTESIAN_POINT('',(-400.,261.,-12.7));
#21401=CARTESIAN_POINT('',(-400.,-261.,-12.7));
#21402=CARTESIAN_POINT('',(-400.,261.,-12.7));
#21403=CARTESIAN_POINT('',(-412.7,261.,-12.7));
#21404=CARTESIAN_POINT('',(-412.7,261.,-12.7));
#21405=CARTESIAN_POINT('',(-412.7,-261.,-12.7));
#21406=CARTESIAN_POINT('',(-412.7,261.,-12.7));
#21407=CARTESIAN_POINT('',(-412.7,-261.,-12.7));
#21408=CARTESIAN_POINT('Origin',(-412.7,-261.,-589.215307716505));
#21409=CARTESIAN_POINT('',(-400.,-261.,-589.215307716505));
#21410=CARTESIAN_POINT('',(-400.,-261.,-589.215307716505));
#21411=CARTESIAN_POINT('',(-412.7,-261.,-589.215307716505));
#21412=CARTESIAN_POINT('',(-412.7,-261.,-589.215307716505));
#21413=CARTESIAN_POINT('',(-412.7,-261.,-589.215307716505));
#21414=CARTESIAN_POINT('Origin',(-412.7,-276.,-662.7));
#21415=CARTESIAN_POINT('',(-400.,-201.,-662.7));
#21416=CARTESIAN_POINT('Origin',(-400.,-276.,-662.7));
#21417=CARTESIAN_POINT('',(-412.7,-201.,-662.7));
#21418=CARTESIAN_POINT('Origin',(-412.7,-276.,-662.7));
#21419=CARTESIAN_POINT('',(-412.7,-201.,-662.7));
#21420=CARTESIAN_POINT('Origin',(-412.7,-201.,-1012.7));
#21421=CARTESIAN_POINT('',(-400.,-201.,-1012.7));
#21422=CARTESIAN_POINT('',(-400.,-201.,-1012.7));
#21423=CARTESIAN_POINT('',(-412.7,-201.,-1012.7));
#21424=CARTESIAN_POINT('',(-412.7,-201.,-1012.7));
#21425=CARTESIAN_POINT('',(-412.7,-201.,-1012.7));
#21426=CARTESIAN_POINT('Origin',(-412.7,261.,-1012.7));
#21427=CARTESIAN_POINT('',(-400.,261.,-1012.7));
#21428=CARTESIAN_POINT('',(-400.,261.,-1012.7));
#21429=CARTESIAN_POINT('',(-412.7,261.,-1012.7));
#21430=CARTESIAN_POINT('',(-412.7,261.,-1012.7));
#21431=CARTESIAN_POINT('',(-412.7,261.,-1012.7));
#21432=CARTESIAN_POINT('Origin',(-412.7,261.,-12.7));
#21433=CARTESIAN_POINT('',(-400.,261.,-12.7));
#21434=CARTESIAN_POINT('',(-412.7,261.,-12.7));
#21435=CARTESIAN_POINT('Origin',(-412.7,-276.,-662.7));
#21436=CARTESIAN_POINT('Origin',(-400.,-276.,-662.7));
#21437=CARTESIAN_POINT('Origin',(442.5,276.875,30.));
#21438=CARTESIAN_POINT('',(442.5,276.875,39.));
#21439=CARTESIAN_POINT('Origin',(442.5,276.875,30.));
#21440=CARTESIAN_POINT('',(442.5,261.,39.));
#21441=CARTESIAN_POINT('',(442.5,276.875,39.));
#21442=CARTESIAN_POINT('Origin',(442.5,261.,30.));
#21443=CARTESIAN_POINT('Origin',(265.5,276.875,30.));
#21444=CARTESIAN_POINT('',(265.5,276.875,39.));
#21445=CARTESIAN_POINT('Origin',(265.5,276.875,30.));
#21446=CARTESIAN_POINT('',(265.5,261.,39.));
#21447=CARTESIAN_POINT('',(265.5,276.875,39.));
#21448=CARTESIAN_POINT('Origin',(265.5,261.,30.));
#21449=CARTESIAN_POINT('Origin',(88.4999999999999,276.875,30.));
#21450=CARTESIAN_POINT('',(88.4999999999999,276.875,39.));
#21451=CARTESIAN_POINT('Origin',(88.4999999999999,276.875,30.));
#21452=CARTESIAN_POINT('',(88.4999999999999,261.,39.));
#21453=CARTESIAN_POINT('',(88.4999999999999,276.875,39.));
#21454=CARTESIAN_POINT('Origin',(88.4999999999999,261.,30.));
#21455=CARTESIAN_POINT('Origin',(-88.5,276.875,30.));
#21456=CARTESIAN_POINT('',(-88.5,276.875,39.));
#21457=CARTESIAN_POINT('Origin',(-88.5,276.875,30.));
#21458=CARTESIAN_POINT('',(-88.5,261.,39.));
#21459=CARTESIAN_POINT('',(-88.5,276.875,39.));
#21460=CARTESIAN_POINT('Origin',(-88.5,261.,30.));
#21461=CARTESIAN_POINT('Origin',(-265.5,276.875,30.));
#21462=CARTESIAN_POINT('',(-265.5,276.875,39.));
#21463=CARTESIAN_POINT('Origin',(-265.5,276.875,30.));
#21464=CARTESIAN_POINT('',(-265.5,261.,39.));
#21465=CARTESIAN_POINT('',(-265.5,276.875,39.));
#21466=CARTESIAN_POINT('Origin',(-265.5,261.,30.));
#21467=CARTESIAN_POINT('Origin',(-442.5,276.875,30.));
#21468=CARTESIAN_POINT('',(-442.5,276.875,39.));
#21469=CARTESIAN_POINT('Origin',(-442.5,276.875,30.));
#21470=CARTESIAN_POINT('',(-442.5,261.,39.));
#21471=CARTESIAN_POINT('',(-442.5,276.875,39.));
#21472=CARTESIAN_POINT('Origin',(-442.5,261.,30.));
#21473=CARTESIAN_POINT('Origin',(0.,276.875,0.));
#21474=CARTESIAN_POINT('',(-463.5,276.875,0.));
#21475=CARTESIAN_POINT('',(-463.5,276.875,51.));
#21476=CARTESIAN_POINT('',(-463.5,276.875,0.));
#21477=CARTESIAN_POINT('',(463.5,276.875,50.9999999999998));
#21478=CARTESIAN_POINT('',(-463.5,276.875,51.));
#21479=CARTESIAN_POINT('',(463.5,276.875,-1.70287137421439E-13));
#21480=CARTESIAN_POINT('',(463.5,276.875,-1.70287137421439E-13));
#21481=CARTESIAN_POINT('',(-463.5,276.875,0.));
#21482=CARTESIAN_POINT('Origin',(0.,261.,0.));
#21483=CARTESIAN_POINT('',(-463.5,261.,0.));
#21484=CARTESIAN_POINT('',(-463.5,261.,51.));
#21485=CARTESIAN_POINT('',(-463.5,261.,0.));
#21486=CARTESIAN_POINT('',(463.5,261.,-1.70287137421439E-13));
#21487=CARTESIAN_POINT('',(-463.5,261.,0.));
#21488=CARTESIAN_POINT('',(463.5,261.,50.9999999999998));
#21489=CARTESIAN_POINT('',(463.5,261.,-1.70287137421439E-13));
#21490=CARTESIAN_POINT('',(-463.5,261.,51.));
#21491=CARTESIAN_POINT('Origin',(-463.5,276.875,0.));
#21492=CARTESIAN_POINT('',(-463.5,276.875,51.));
#21493=CARTESIAN_POINT('',(-463.5,276.875,0.));
#21494=CARTESIAN_POINT('Origin',(-463.5,276.875,51.));
#21495=CARTESIAN_POINT('',(463.5,276.875,50.9999999999998));
#21496=CARTESIAN_POINT('Origin',(463.5,276.875,-1.70287137421439E-13));
#21497=CARTESIAN_POINT('',(463.5,276.875,-1.70287137421439E-13));
#21498=CARTESIAN_POINT('Origin',(-463.5,276.875,0.));
#21499=CARTESIAN_POINT('Origin',(-442.5,261.,-170.));
#21500=CARTESIAN_POINT('',(-442.5,261.,-179.));
#21501=CARTESIAN_POINT('Origin',(-442.5,261.,-170.));
#21502=CARTESIAN_POINT('',(-442.5,276.875,-179.));
#21503=CARTESIAN_POINT('',(-442.5,261.,-179.));
#21504=CARTESIAN_POINT('Origin',(-442.5,276.875,-170.));
#21505=CARTESIAN_POINT('Origin',(-442.499999999994,261.,-370.175));
#21506=CARTESIAN_POINT('',(-442.499999999994,261.,-379.175));
#21507=CARTESIAN_POINT('Origin',(-442.499999999994,261.,-370.175));
#21508=CARTESIAN_POINT('',(-442.499999999994,276.875,-379.175));
#21509=CARTESIAN_POINT('',(-442.499999999994,261.,-379.175));
#21510=CARTESIAN_POINT('Origin',(-442.499999999994,276.875,-370.175));
#21511=CARTESIAN_POINT('Origin',(-442.499999999996,261.,-570.35));
#21512=CARTESIAN_POINT('',(-442.499999999996,261.,-579.35));
#21513=CARTESIAN_POINT('Origin',(-442.499999999996,261.,-570.35));
#21514=CARTESIAN_POINT('',(-442.499999999996,276.875,-579.35));
#21515=CARTESIAN_POINT('',(-442.499999999996,261.,-579.35));
#21516=CARTESIAN_POINT('Origin',(-442.499999999996,276.875,-570.35));
#21517=CARTESIAN_POINT('Origin',(-442.499999999998,261.,-770.525));
#21518=CARTESIAN_POINT('',(-442.499999999998,261.,-779.525));
#21519=CARTESIAN_POINT('Origin',(-442.499999999998,261.,-770.525));
#21520=CARTESIAN_POINT('',(-442.499999999998,276.875,-779.525));
#21521=CARTESIAN_POINT('',(-442.499999999998,261.,-779.525));
#21522=CARTESIAN_POINT('Origin',(-442.499999999998,276.875,-770.525));
#21523=CARTESIAN_POINT('Origin',(-442.5,261.,-970.7));
#21524=CARTESIAN_POINT('',(-442.5,261.,-979.7));
#21525=CARTESIAN_POINT('Origin',(-442.5,261.,-970.7));
#21526=CARTESIAN_POINT('',(-442.5,276.875,-979.7));
#21527=CARTESIAN_POINT('',(-442.5,261.,-979.7));
#21528=CARTESIAN_POINT('Origin',(-442.5,276.875,-970.7));
#21529=CARTESIAN_POINT('Origin',(-463.5,261.,0.));
#21530=CARTESIAN_POINT('',(-463.5,276.875,-1012.7));
#21531=CARTESIAN_POINT('',(-463.5,276.875,0.));
#21532=CARTESIAN_POINT('',(-463.5,276.875,0.));
#21533=CARTESIAN_POINT('',(-463.5,261.,-1012.7));
#21534=CARTESIAN_POINT('',(-463.5,261.,-1012.7));
#21535=CARTESIAN_POINT('',(-463.5,261.,0.));
#21536=CARTESIAN_POINT('',(-463.5,261.,0.));
#21537=CARTESIAN_POINT('',(-463.5,261.,0.));
#21538=CARTESIAN_POINT('Origin',(-463.5,261.,-1012.7));
#21539=CARTESIAN_POINT('',(-412.7,276.875,-1012.7));
#21540=CARTESIAN_POINT('',(-463.5,276.875,-1012.7));
#21541=CARTESIAN_POINT('',(-412.7,261.,-1012.7));
#21542=CARTESIAN_POINT('',(-412.7,261.,-1012.7));
#21543=CARTESIAN_POINT('',(-463.5,261.,-1012.7));
#21544=CARTESIAN_POINT('Origin',(-412.7,261.,0.));
#21545=CARTESIAN_POINT('',(-412.7,276.875,0.));
#21546=CARTESIAN_POINT('',(-412.7,276.875,0.));
#21547=CARTESIAN_POINT('',(-412.7,261.,0.));
#21548=CARTESIAN_POINT('',(-412.7,261.,0.));
#21549=CARTESIAN_POINT('',(-412.7,261.,0.));
#21550=CARTESIAN_POINT('Origin',(-463.5,261.,0.));
#21551=CARTESIAN_POINT('',(-463.5,276.875,0.));
#21552=CARTESIAN_POINT('',(-463.5,261.,0.));
#21553=CARTESIAN_POINT('Origin',(0.,261.,0.));
#21554=CARTESIAN_POINT('Origin',(0.,276.875,0.));
#21555=CARTESIAN_POINT('Origin',(442.5,261.,-170.));
#21556=CARTESIAN_POINT('',(442.5,261.,-179.));
#21557=CARTESIAN_POINT('Origin',(442.5,261.,-170.));
#21558=CARTESIAN_POINT('',(442.5,276.875,-179.));
#21559=CARTESIAN_POINT('',(442.5,261.,-179.));
#21560=CARTESIAN_POINT('Origin',(442.5,276.875,-170.));
#21561=CARTESIAN_POINT('Origin',(442.499999999994,261.,-370.175));
#21562=CARTESIAN_POINT('',(442.499999999994,261.,-379.175));
#21563=CARTESIAN_POINT('Origin',(442.499999999994,261.,-370.175));
#21564=CARTESIAN_POINT('',(442.499999999994,276.875,-379.175));
#21565=CARTESIAN_POINT('',(442.499999999994,261.,-379.175));
#21566=CARTESIAN_POINT('Origin',(442.499999999994,276.875,-370.175));
#21567=CARTESIAN_POINT('Origin',(442.499999999996,261.,-570.35));
#21568=CARTESIAN_POINT('',(442.499999999996,261.,-579.35));
#21569=CARTESIAN_POINT('Origin',(442.499999999996,261.,-570.35));
#21570=CARTESIAN_POINT('',(442.499999999996,276.875,-579.35));
#21571=CARTESIAN_POINT('',(442.499999999996,261.,-579.35));
#21572=CARTESIAN_POINT('Origin',(442.499999999996,276.875,-570.35));
#21573=CARTESIAN_POINT('Origin',(442.499999999998,261.,-770.525));
#21574=CARTESIAN_POINT('',(442.499999999998,261.,-779.525));
#21575=CARTESIAN_POINT('Origin',(442.499999999998,261.,-770.525));
#21576=CARTESIAN_POINT('',(442.499999999998,276.875,-779.525));
#21577=CARTESIAN_POINT('',(442.499999999998,261.,-779.525));
#21578=CARTESIAN_POINT('Origin',(442.499999999998,276.875,-770.525));
#21579=CARTESIAN_POINT('Origin',(442.5,261.,-970.7));
#21580=CARTESIAN_POINT('',(442.5,261.,-979.7));
#21581=CARTESIAN_POINT('Origin',(442.5,261.,-970.7));
#21582=CARTESIAN_POINT('',(442.5,276.875,-979.7));
#21583=CARTESIAN_POINT('',(442.5,261.,-979.7));
#21584=CARTESIAN_POINT('Origin',(442.5,276.875,-970.7));
#21585=CARTESIAN_POINT('Origin',(463.5,261.,0.));
#21586=CARTESIAN_POINT('',(463.5,276.875,-1012.7));
#21587=CARTESIAN_POINT('',(463.5,276.875,0.));
#21588=CARTESIAN_POINT('',(463.5,276.875,0.));
#21589=CARTESIAN_POINT('',(463.5,261.,0.));
#21590=CARTESIAN_POINT('',(463.5,261.,0.));
#21591=CARTESIAN_POINT('',(463.5,261.,-1012.7));
#21592=CARTESIAN_POINT('',(463.5,261.,0.));
#21593=CARTESIAN_POINT('',(463.5,261.,-1012.7));
#21594=CARTESIAN_POINT('Origin',(463.5,261.,-1012.7));
#21595=CARTESIAN_POINT('',(412.7,276.875,-1012.7));
#21596=CARTESIAN_POINT('',(463.5,276.875,-1012.7));
#21597=CARTESIAN_POINT('',(412.7,261.,-1012.7));
#21598=CARTESIAN_POINT('',(463.5,261.,-1012.7));
#21599=CARTESIAN_POINT('',(412.7,261.,-1012.7));
#21600=CARTESIAN_POINT('Origin',(412.7,261.,0.));
#21601=CARTESIAN_POINT('',(412.7,276.875,0.));
#21602=CARTESIAN_POINT('',(412.7,276.875,0.));
#21603=CARTESIAN_POINT('',(412.7,261.,0.));
#21604=CARTESIAN_POINT('',(412.7,261.,0.));
#21605=CARTESIAN_POINT('',(412.7,261.,0.));
#21606=CARTESIAN_POINT('Origin',(463.5,261.,0.));
#21607=CARTESIAN_POINT('',(463.5,276.875,0.));
#21608=CARTESIAN_POINT('',(463.5,261.,0.));
#21609=CARTESIAN_POINT('Origin',(0.,261.,0.));
#21610=CARTESIAN_POINT('Origin',(0.,276.875,0.));
#21611=CARTESIAN_POINT('Origin',(463.5,-276.875,50.9999999999998));
#21612=CARTESIAN_POINT('',(463.5,-261.,50.9999999999998));
#21613=CARTESIAN_POINT('',(-463.5,-261.,51.));
#21614=CARTESIAN_POINT('',(463.5,-261.,50.9999999999998));
#21615=CARTESIAN_POINT('',(-463.5,-276.875,51.));
#21616=CARTESIAN_POINT('',(-463.5,-276.875,51.));
#21617=CARTESIAN_POINT('',(463.5,-276.875,50.9999999999998));
#21618=CARTESIAN_POINT('',(463.5,-276.875,50.9999999999998));
#21619=CARTESIAN_POINT('',(463.5,-276.875,50.9999999999998));
#21620=CARTESIAN_POINT('Origin',(-463.5,-276.875,51.));
#21621=CARTESIAN_POINT('',(-463.5,-261.,0.));
#21622=CARTESIAN_POINT('',(-463.5,-261.,51.));
#21623=CARTESIAN_POINT('',(-463.5,-276.875,0.));
#21624=CARTESIAN_POINT('',(-463.5,-276.875,0.));
#21625=CARTESIAN_POINT('',(-463.5,-276.875,51.));
#21626=CARTESIAN_POINT('Origin',(-463.5,-276.875,0.));
#21627=CARTESIAN_POINT('',(463.5,-261.,-1.70287137421439E-13));
#21628=CARTESIAN_POINT('',(-463.5,-261.,0.));
#21629=CARTESIAN_POINT('',(463.5,-276.875,-1.70287137421439E-13));
#21630=CARTESIAN_POINT('',(463.5,-276.875,-1.70287137421439E-13));
#21631=CARTESIAN_POINT('',(-463.5,-276.875,0.));
#21632=CARTESIAN_POINT('Origin',(463.5,-276.875,-1.70287137421439E-13));
#21633=CARTESIAN_POINT('',(463.5,-261.,-1.70287137421439E-13));
#21634=CARTESIAN_POINT('',(463.5,-276.875,-1.70287137421439E-13));
#21635=CARTESIAN_POINT('Origin',(0.,-276.875,0.));
#21636=CARTESIAN_POINT('Origin',(0.,-261.,0.));
#21637=CARTESIAN_POINT('Origin',(463.5,-276.875,-5.17905770564469E-14));
#21638=CARTESIAN_POINT('',(463.5,-261.,-469.));
#21639=CARTESIAN_POINT('',(463.5,-261.,-5.02620148240116E-14));
#21640=CARTESIAN_POINT('',(463.5,-261.,-5.02620148240116E-14));
#21641=CARTESIAN_POINT('',(463.5,-276.875,-5.17905770564469E-14));
#21642=CARTESIAN_POINT('',(463.5,-276.875,-5.17905770564469E-14));
#21643=CARTESIAN_POINT('',(463.5,-276.875,-469.));
#21644=CARTESIAN_POINT('',(463.5,-276.875,-5.17905770564469E-14));
#21645=CARTESIAN_POINT('',(463.5,-276.875,-469.));
#21646=CARTESIAN_POINT('Origin',(463.5,-276.875,-5.17905770564469E-14));
#21647=CARTESIAN_POINT('',(412.7,-261.,-3.13522131516744E-14));
#21648=CARTESIAN_POINT('',(463.5,-261.,-5.02620148240116E-14));
#21649=CARTESIAN_POINT('',(412.7,-276.875,-3.28807753841096E-14));
#21650=CARTESIAN_POINT('',(412.7,-276.875,-3.28807753841096E-14));
#21651=CARTESIAN_POINT('',(463.5,-276.875,-5.17905770564469E-14));
#21652=CARTESIAN_POINT('Origin',(412.7,-276.875,-3.28807753841096E-14));
#21653=CARTESIAN_POINT('',(412.7,-261.,-469.));
#21654=CARTESIAN_POINT('',(412.7,-261.,-3.13522131516744E-14));
#21655=CARTESIAN_POINT('',(412.7,-276.875,-469.));
#21656=CARTESIAN_POINT('',(412.7,-276.875,-469.));
#21657=CARTESIAN_POINT('',(412.7,-276.875,-3.28807753841096E-14));
#21658=CARTESIAN_POINT('Origin',(463.5,-276.875,-469.));
#21659=CARTESIAN_POINT('',(463.5,-261.,-469.));
#21660=CARTESIAN_POINT('',(463.5,-276.875,-469.));
#21661=CARTESIAN_POINT('Origin',(0.,-276.875,-3.24206954336256E-14));
#21662=CARTESIAN_POINT('Origin',(0.,-261.,-3.08921332011904E-14));
#21663=CARTESIAN_POINT('Origin',(-463.5,-276.875,-5.17905770564469E-14));
#21664=CARTESIAN_POINT('',(-463.5,-261.,-469.));
#21665=CARTESIAN_POINT('',(-463.5,-261.,-5.02620148240116E-14));
#21666=CARTESIAN_POINT('',(-463.5,-261.,-5.02620148240116E-14));
#21667=CARTESIAN_POINT('',(-463.5,-276.875,-469.));
#21668=CARTESIAN_POINT('',(-463.5,-276.875,-469.));
#21669=CARTESIAN_POINT('',(-463.5,-276.875,-5.17905770564469E-14));
#21670=CARTESIAN_POINT('',(-463.5,-276.875,-5.17905770564469E-14));
#21671=CARTESIAN_POINT('',(-463.5,-276.875,-5.17905770564469E-14));
#21672=CARTESIAN_POINT('Origin',(-463.5,-276.875,-5.17905770564469E-14));
#21673=CARTESIAN_POINT('',(-412.7,-261.,-3.13522131516744E-14));
#21674=CARTESIAN_POINT('',(-463.5,-261.,-5.02620148240116E-14));
#21675=CARTESIAN_POINT('',(-412.7,-276.875,-3.28807753841096E-14));
#21676=CARTESIAN_POINT('',(-463.5,-276.875,-5.17905770564469E-14));
#21677=CARTESIAN_POINT('',(-412.7,-276.875,-3.28807753841096E-14));
#21678=CARTESIAN_POINT('Origin',(-412.7,-276.875,-3.28807753841096E-14));
#21679=CARTESIAN_POINT('',(-412.7,-261.,-469.));
#21680=CARTESIAN_POINT('',(-412.7,-261.,-3.13522131516744E-14));
#21681=CARTESIAN_POINT('',(-412.7,-276.875,-469.));
#21682=CARTESIAN_POINT('',(-412.7,-276.875,-3.28807753841096E-14));
#21683=CARTESIAN_POINT('',(-412.7,-276.875,-469.));
#21684=CARTESIAN_POINT('Origin',(-463.5,-276.875,-469.));
#21685=CARTESIAN_POINT('',(-463.5,-261.,-469.));
#21686=CARTESIAN_POINT('',(-463.5,-276.875,-469.));
#21687=CARTESIAN_POINT('Origin',(0.,-276.875,-3.24206954336256E-14));
#21688=CARTESIAN_POINT('Origin',(0.,-261.,-3.08921332011904E-14));
#21689=CARTESIAN_POINT('',(0.,0.,0.));
#21690=CARTESIAN_POINT('Origin',(-510.49999999999,-7.9375000000001,442.500000000001));
#21691=CARTESIAN_POINT('',(-510.49999999999,-7.9375000000001,433.500000000001));
#21692=CARTESIAN_POINT('Origin',(-510.49999999999,-7.9375000000001,442.500000000001));
#21693=CARTESIAN_POINT('',(-510.49999999999,-5.88418203051333E-14,433.500000000001));
#21694=CARTESIAN_POINT('',(-510.49999999999,-7.9375000000001,433.500000000001));
#21695=CARTESIAN_POINT('Origin',(-510.49999999999,-5.55111512312578E-14,
442.500000000001));
#21696=CARTESIAN_POINT('Origin',(-510.499999999992,-7.9375000000001,265.5));
#21697=CARTESIAN_POINT('',(-510.499999999992,-7.9375000000001,256.5));
#21698=CARTESIAN_POINT('Origin',(-510.499999999992,-7.9375000000001,265.5));
#21699=CARTESIAN_POINT('',(-510.499999999992,-5.88418203051333E-14,256.5));
#21700=CARTESIAN_POINT('',(-510.499999999992,-7.9375000000001,256.5));
#21701=CARTESIAN_POINT('Origin',(-510.499999999992,-5.55111512312578E-14,
265.5));
#21702=CARTESIAN_POINT('Origin',(-510.499999999994,-7.93750000000004,88.5000000000001));
#21703=CARTESIAN_POINT('',(-510.499999999994,-7.93750000000005,79.5000000000001));
#21704=CARTESIAN_POINT('Origin',(-510.499999999994,-7.93750000000004,88.5000000000001));
#21705=CARTESIAN_POINT('',(-510.499999999994,-3.33066907387547E-15,79.5000000000001));
#21706=CARTESIAN_POINT('',(-510.499999999994,-7.93750000000005,79.5000000000001));
#21707=CARTESIAN_POINT('Origin',(-510.499999999994,0.,88.5000000000001));
#21708=CARTESIAN_POINT('Origin',(-510.499999999996,-7.93750000000004,-88.5));
#21709=CARTESIAN_POINT('',(-510.499999999996,-7.93750000000005,-97.5000000000001));
#21710=CARTESIAN_POINT('Origin',(-510.499999999996,-7.93750000000004,-88.5));
#21711=CARTESIAN_POINT('',(-510.499999999996,-3.33066907387547E-15,-97.5000000000001));
#21712=CARTESIAN_POINT('',(-510.499999999996,-7.93750000000005,-97.5000000000001));
#21713=CARTESIAN_POINT('Origin',(-510.499999999996,0.,-88.5));
#21714=CARTESIAN_POINT('Origin',(-510.499999999998,-7.93749999999999,-265.5));
#21715=CARTESIAN_POINT('',(-510.499999999998,-7.93749999999999,-274.5));
#21716=CARTESIAN_POINT('Origin',(-510.499999999998,-7.93749999999999,-265.5));
#21717=CARTESIAN_POINT('',(-510.499999999998,5.21804821573824E-14,-274.5));
#21718=CARTESIAN_POINT('',(-510.499999999998,-7.93749999999999,-274.5));
#21719=CARTESIAN_POINT('Origin',(-510.499999999998,5.55111512312578E-14,
-265.5));
#21720=CARTESIAN_POINT('Origin',(489.50000000001,-7.9375000000001,442.499999999987));
#21721=CARTESIAN_POINT('',(489.50000000001,-7.9375000000001,433.499999999987));
#21722=CARTESIAN_POINT('Origin',(489.50000000001,-7.9375000000001,442.499999999987));
#21723=CARTESIAN_POINT('',(489.50000000001,-5.88418203051333E-14,433.499999999987));
#21724=CARTESIAN_POINT('',(489.50000000001,-7.9375000000001,433.499999999987));
#21725=CARTESIAN_POINT('Origin',(489.50000000001,-5.55111512312578E-14,
442.499999999987));
#21726=CARTESIAN_POINT('Origin',(289.50000000001,-7.9375000000001,442.49999999999));
#21727=CARTESIAN_POINT('',(289.50000000001,-7.9375000000001,433.499999999989));
#21728=CARTESIAN_POINT('Origin',(289.50000000001,-7.9375000000001,442.49999999999));
#21729=CARTESIAN_POINT('',(289.50000000001,-5.88418203051333E-14,433.499999999989));
#21730=CARTESIAN_POINT('',(289.50000000001,-7.9375000000001,433.499999999989));
#21731=CARTESIAN_POINT('Origin',(289.50000000001,-5.55111512312578E-14,
442.49999999999));
#21732=CARTESIAN_POINT('Origin',(89.5000000000096,-7.9375000000001,442.499999999992));
#21733=CARTESIAN_POINT('',(89.5000000000096,-7.9375000000001,433.499999999992));
#21734=CARTESIAN_POINT('Origin',(89.5000000000096,-7.9375000000001,442.499999999992));
#21735=CARTESIAN_POINT('',(89.5000000000096,-5.88418203051333E-14,433.499999999992));
#21736=CARTESIAN_POINT('',(89.5000000000096,-7.9375000000001,433.499999999992));
#21737=CARTESIAN_POINT('Origin',(89.5000000000096,-5.55111512312578E-14,
442.499999999992));
#21738=CARTESIAN_POINT('Origin',(-110.49999999999,-7.9375000000001,442.499999999995));
#21739=CARTESIAN_POINT('',(-110.49999999999,-7.9375000000001,433.499999999995));
#21740=CARTESIAN_POINT('Origin',(-110.49999999999,-7.9375000000001,442.499999999995));
#21741=CARTESIAN_POINT('',(-110.49999999999,-5.88418203051333E-14,433.499999999995));
#21742=CARTESIAN_POINT('',(-110.49999999999,-7.9375000000001,433.499999999995));
#21743=CARTESIAN_POINT('Origin',(-110.49999999999,-5.55111512312578E-14,
442.499999999995));
#21744=CARTESIAN_POINT('Origin',(-310.499999999991,-7.9375000000001,442.499999999998));
#21745=CARTESIAN_POINT('',(-310.499999999991,-7.9375000000001,433.499999999998));
#21746=CARTESIAN_POINT('Origin',(-310.499999999991,-7.9375000000001,442.499999999998));
#21747=CARTESIAN_POINT('',(-310.499999999991,-5.88418203051333E-14,433.499999999998));
#21748=CARTESIAN_POINT('',(-310.499999999991,-7.9375000000001,433.499999999998));
#21749=CARTESIAN_POINT('Origin',(-310.499999999991,-5.55111512312578E-14,
442.499999999998));
#21750=CARTESIAN_POINT('Origin',(489.500000000001,-7.93749999999999,-442.500000000001));
#21751=CARTESIAN_POINT('',(489.500000000001,-7.93749999999999,-451.500000000005));
#21752=CARTESIAN_POINT('Origin',(489.500000000001,-7.93749999999999,-442.500000000001));
#21753=CARTESIAN_POINT('',(489.500000000001,5.21804821573824E-14,-451.500000000005));
#21754=CARTESIAN_POINT('',(489.500000000001,-7.93749999999999,-451.500000000005));
#21755=CARTESIAN_POINT('Origin',(489.500000000001,5.55111512312578E-14,
-442.500000000001));
#21756=CARTESIAN_POINT('Origin',(289.5,-7.93749999999999,-442.500000000012));
#21757=CARTESIAN_POINT('',(289.5,-7.93749999999999,-451.500000000012));
#21758=CARTESIAN_POINT('Origin',(289.5,-7.93749999999999,-442.500000000012));
#21759=CARTESIAN_POINT('',(289.5,5.21804821573824E-14,-451.500000000012));
#21760=CARTESIAN_POINT('',(289.5,-7.93749999999999,-451.500000000012));
#21761=CARTESIAN_POINT('Origin',(289.5,5.55111512312578E-14,-442.500000000012));
#21762=CARTESIAN_POINT('Origin',(89.5000000000004,-7.93749999999999,-442.500000000009));
#21763=CARTESIAN_POINT('',(89.5000000000004,-7.93749999999999,-451.500000000009));
#21764=CARTESIAN_POINT('Origin',(89.5000000000004,-7.93749999999999,-442.500000000009));
#21765=CARTESIAN_POINT('',(89.5000000000004,5.21804821573824E-14,-451.500000000009));
#21766=CARTESIAN_POINT('',(89.5000000000004,-7.93749999999999,-451.500000000009));
#21767=CARTESIAN_POINT('Origin',(89.5000000000004,5.55111512312578E-14,
-442.500000000009));
#21768=CARTESIAN_POINT('Origin',(-110.5,-7.93749999999999,-442.500000000006));
#21769=CARTESIAN_POINT('',(-110.5,-7.93749999999999,-451.500000000006));
#21770=CARTESIAN_POINT('Origin',(-110.5,-7.93749999999999,-442.500000000006));
#21771=CARTESIAN_POINT('',(-110.5,5.21804821573824E-14,-451.500000000006));
#21772=CARTESIAN_POINT('',(-110.5,-7.93749999999999,-451.500000000006));
#21773=CARTESIAN_POINT('Origin',(-110.5,5.55111512312578E-14,-442.500000000006));
#21774=CARTESIAN_POINT('Origin',(-310.5,-7.93749999999999,-442.500000000003));
#21775=CARTESIAN_POINT('',(-310.5,-7.93749999999999,-451.500000000003));
#21776=CARTESIAN_POINT('Origin',(-310.5,-7.93749999999999,-442.500000000003));
#21777=CARTESIAN_POINT('',(-310.5,5.21804821573824E-14,-451.500000000003));
#21778=CARTESIAN_POINT('',(-310.5,-7.93749999999999,-451.500000000003));
#21779=CARTESIAN_POINT('Origin',(-310.5,5.55111512312578E-14,-442.500000000003));
#21780=CARTESIAN_POINT('Origin',(-278.5,-7.93749999999999,-300.));
#21781=CARTESIAN_POINT('',(-278.5,-7.9375,-331.000000000001));
#21782=CARTESIAN_POINT('Origin',(-278.5,-7.93749999999999,-300.));
#21783=CARTESIAN_POINT('',(-278.5,4.66293670342566E-14,-331.000000000001));
#21784=CARTESIAN_POINT('',(-278.5,-7.9375,-331.000000000001));
#21785=CARTESIAN_POINT('Origin',(-278.5,5.55111512312578E-14,-300.));
#21786=CARTESIAN_POINT('Origin',(-278.5,-7.93750000000004,2.64371857738874E-15));
#21787=CARTESIAN_POINT('',(-278.5,-7.93750000000009,-138.));
#21788=CARTESIAN_POINT('Origin',(-278.5,-7.93750000000004,2.64371857738874E-15));
#21789=CARTESIAN_POINT('',(-278.5,-4.55191440096314E-14,-138.));
#21790=CARTESIAN_POINT('',(-278.5,-7.93750000000009,-138.));
#21791=CARTESIAN_POINT('Origin',(-278.5,0.,7.39557098644699E-29));
#21792=CARTESIAN_POINT('Origin',(-510.5,-7.93749999999999,-442.500000000001));
#21793=CARTESIAN_POINT('',(-510.5,-7.93749999999999,-451.500000000001));
#21794=CARTESIAN_POINT('Origin',(-510.5,-7.93749999999999,-442.500000000001));
#21795=CARTESIAN_POINT('',(-510.5,5.21804821573824E-14,-451.500000000001));
#21796=CARTESIAN_POINT('',(-510.5,-7.93749999999999,-451.500000000001));
#21797=CARTESIAN_POINT('Origin',(-510.5,5.55111512312578E-14,-442.500000000001));
#21798=CARTESIAN_POINT('Origin',(531.5,-7.9375000000001,463.500000000001));
#21799=CARTESIAN_POINT('',(531.5,-5.55111512312578E-14,463.500000000001));
#21800=CARTESIAN_POINT('',(531.5,5.55111512312578E-14,-463.500000000001));
#21801=CARTESIAN_POINT('',(531.5,-5.55111512312578E-14,463.500000000001));
#21802=CARTESIAN_POINT('',(531.5,-7.9375000000001,463.500000000001));
#21803=CARTESIAN_POINT('',(531.5,-7.9375000000001,463.500000000001));
#21804=CARTESIAN_POINT('',(531.5,-7.93749999999999,-463.500000000001));
#21805=CARTESIAN_POINT('',(531.5,-7.9375000000001,463.500000000001));
#21806=CARTESIAN_POINT('',(531.5,-7.93749999999999,-463.500000000001));
#21807=CARTESIAN_POINT('Origin',(-531.5,-7.9375000000001,463.500000000001));
#21808=CARTESIAN_POINT('',(-531.5,-5.55111512312578E-14,463.500000000001));
#21809=CARTESIAN_POINT('',(-531.5,-5.55111512312578E-14,463.500000000001));
#21810=CARTESIAN_POINT('',(-531.5,-7.9375000000001,463.500000000001));
#21811=CARTESIAN_POINT('',(-531.5,-7.9375000000001,463.500000000001));
#21812=CARTESIAN_POINT('',(-531.5,-7.9375000000001,463.500000000001));
#21813=CARTESIAN_POINT('Origin',(-531.5,-7.9375000000001,463.500000000001));
#21814=CARTESIAN_POINT('',(-531.5,5.55111512312578E-14,-463.500000000001));
#21815=CARTESIAN_POINT('',(-531.5,-5.55111512312578E-14,463.500000000001));
#21816=CARTESIAN_POINT('',(-531.5,-7.93749999999999,-463.500000000001));
#21817=CARTESIAN_POINT('',(-531.5,-7.93749999999999,-463.500000000001));
#21818=CARTESIAN_POINT('',(-531.5,-7.9375000000001,463.500000000001));
#21819=CARTESIAN_POINT('Origin',(-531.5,-7.93749999999999,-463.500000000001));
#21820=CARTESIAN_POINT('',(-531.5,5.55111512312578E-14,-463.500000000001));
#21821=CARTESIAN_POINT('',(-531.5,-7.93749999999999,-463.500000000001));
#21822=CARTESIAN_POINT('Origin',(0.,-7.93750000000004,2.6437185773887E-15));
#21823=CARTESIAN_POINT('Origin',(0.,0.,0.));
#21824=CARTESIAN_POINT('Origin',(-278.5,140.,-3.10862446895044E-14));
#21825=CARTESIAN_POINT('',(-278.5,1.77635683940025E-14,136.525));
#21826=CARTESIAN_POINT('Origin',(-278.5,0.,4.93038065763132E-29));
#21827=CARTESIAN_POINT('',(-278.5,140.,136.525));
#21828=CARTESIAN_POINT('',(-278.5,140.,136.525));
#21829=CARTESIAN_POINT('Origin',(-278.5,140.,-3.10862446895044E-14));
#21830=CARTESIAN_POINT('Origin',(-278.5,140.,-3.10862446895044E-14));
#21831=CARTESIAN_POINT('',(-278.5,140.,121.435));
#21832=CARTESIAN_POINT('Origin',(-278.5,140.,-3.10862446895044E-14));
#21833=CARTESIAN_POINT('',(-278.5,0.,121.435));
#21834=CARTESIAN_POINT('',(-278.5,140.,121.435));
#21835=CARTESIAN_POINT('Origin',(-278.5,0.,4.93038065763132E-29));
#21836=CARTESIAN_POINT('Origin',(-278.5,140.,-3.10862446895044E-14));
#21837=CARTESIAN_POINT('Origin',(-278.5,0.,4.93038065763132E-29));
#21838=CARTESIAN_POINT('Origin',(-278.5,232.,-300.));
#21839=CARTESIAN_POINT('',(-308.665,-58.0000000000001,-300.));
#21840=CARTESIAN_POINT('Origin',(-278.5,-58.,-300.));
#21841=CARTESIAN_POINT('',(-308.665,232.,-300.));
#21842=CARTESIAN_POINT('',(-308.665,232.,-300.));
#21843=CARTESIAN_POINT('Origin',(-278.5,232.,-300.));
#21844=CARTESIAN_POINT('Origin',(-278.5,232.,-300.));
#21845=CARTESIAN_POINT('',(-304.755,232.,-300.));
#21846=CARTESIAN_POINT('Origin',(-278.5,232.,-300.));
#21847=CARTESIAN_POINT('',(-304.755,-58.0000000000001,-300.));
#21848=CARTESIAN_POINT('',(-304.755,232.,-300.));
#21849=CARTESIAN_POINT('Origin',(-278.5,-58.,-300.));
#21850=CARTESIAN_POINT('Origin',(-278.5,232.,-300.));
#21851=CARTESIAN_POINT('Origin',(-278.5,-58.,-300.));
#21852=CARTESIAN_POINT('Origin',(-369.,118.3,-156.750598084984));
#21853=CARTESIAN_POINT('',(-369.,118.3,-169.250598084979));
#21854=CARTESIAN_POINT('Origin',(-369.,118.3,-156.750598084984));
#21855=CARTESIAN_POINT('',(-369.,150.,-169.250598084979));
#21856=CARTESIAN_POINT('',(-369.,118.3,-169.250598084979));
#21857=CARTESIAN_POINT('Origin',(-369.,150.,-156.750598084984));
#21858=CARTESIAN_POINT('Origin',(-435.250598084983,118.3,-90.4999999999999));
#21859=CARTESIAN_POINT('',(-435.250598084983,118.3,-102.999999999983));
#21860=CARTESIAN_POINT('Origin',(-435.250598084983,118.3,-90.4999999999999));
#21861=CARTESIAN_POINT('',(-435.250598084983,150.,-102.999999999983));
#21862=CARTESIAN_POINT('',(-435.250598084983,118.3,-102.999999999983));
#21863=CARTESIAN_POINT('Origin',(-435.250598084983,150.,-90.4999999999999));
#21864=CARTESIAN_POINT('Origin',(-459.5,118.3,3.64870602855833E-14));
#21865=CARTESIAN_POINT('',(-459.5,118.3,-12.4999999999698));
#21866=CARTESIAN_POINT('Origin',(-459.5,118.3,3.64870602855833E-14));
#21867=CARTESIAN_POINT('',(-459.5,150.,-12.4999999999698));
#21868=CARTESIAN_POINT('',(-459.5,118.3,-12.4999999999698));
#21869=CARTESIAN_POINT('Origin',(-459.5,150.,3.13893114861083E-14));
#21870=CARTESIAN_POINT('Origin',(-435.250598084983,118.3,90.5000000000001));
#21871=CARTESIAN_POINT('',(-435.250598084983,118.3,78.0000000000418));
#21872=CARTESIAN_POINT('Origin',(-435.250598084983,118.3,90.5000000000001));
#21873=CARTESIAN_POINT('',(-435.250598084983,150.,78.0000000000418));
#21874=CARTESIAN_POINT('',(-435.250598084983,118.3,78.0000000000418));
#21875=CARTESIAN_POINT('Origin',(-435.250598084983,150.,90.5000000000001));
#21876=CARTESIAN_POINT('Origin',(-369.,118.3,156.750598084983));
#21877=CARTESIAN_POINT('',(-369.,118.3,144.250598085032));
#21878=CARTESIAN_POINT('Origin',(-369.,118.3,156.750598084983));
#21879=CARTESIAN_POINT('',(-369.,150.,144.250598085032));
#21880=CARTESIAN_POINT('',(-369.,118.3,144.250598085032));
#21881=CARTESIAN_POINT('Origin',(-369.,150.,156.750598084983));
#21882=CARTESIAN_POINT('Origin',(-278.5,118.3,181.));
#21883=CARTESIAN_POINT('',(-278.5,118.3,168.500000000048));
#21884=CARTESIAN_POINT('Origin',(-278.5,118.3,181.));
#21885=CARTESIAN_POINT('',(-278.5,150.,168.500000000048));
#21886=CARTESIAN_POINT('',(-278.5,118.3,168.500000000048));
#21887=CARTESIAN_POINT('Origin',(-278.5,150.,181.));
#21888=CARTESIAN_POINT('Origin',(-188.,118.3,156.750598084983));
#21889=CARTESIAN_POINT('',(-188.,118.3,144.250598085024));
#21890=CARTESIAN_POINT('Origin',(-188.,118.3,156.750598084983));
#21891=CARTESIAN_POINT('',(-188.,150.,144.250598085024));
#21892=CARTESIAN_POINT('',(-188.,118.3,144.250598085024));
#21893=CARTESIAN_POINT('Origin',(-188.,150.,156.750598084983));
#21894=CARTESIAN_POINT('Origin',(-121.749401915016,118.3,90.5));
#21895=CARTESIAN_POINT('',(-121.749401915016,118.3,78.0000000000295));
#21896=CARTESIAN_POINT('Origin',(-121.749401915016,118.3,90.5));
#21897=CARTESIAN_POINT('',(-121.749401915016,150.,78.0000000000295));
#21898=CARTESIAN_POINT('',(-121.749401915016,118.3,78.0000000000295));
#21899=CARTESIAN_POINT('Origin',(-121.749401915016,150.,90.5));
#21900=CARTESIAN_POINT('Origin',(-97.4999999999999,118.3,-1.90240909456746E-14));
#21901=CARTESIAN_POINT('',(-97.4999999999999,118.3,-12.4999999999835));
#21902=CARTESIAN_POINT('Origin',(-97.4999999999999,118.3,-1.90240909456746E-14));
#21903=CARTESIAN_POINT('',(-97.4999999999999,150.,-12.4999999999835));
#21904=CARTESIAN_POINT('',(-97.4999999999999,118.3,-12.4999999999835));
#21905=CARTESIAN_POINT('Origin',(-97.4999999999999,150.,-2.41218397451495E-14));
#21906=CARTESIAN_POINT('Origin',(-121.749401915016,118.3,-90.5000000000001));
#21907=CARTESIAN_POINT('',(-121.749401915016,118.3,-102.999999999995));
#21908=CARTESIAN_POINT('Origin',(-121.749401915016,118.3,-90.5000000000001));
#21909=CARTESIAN_POINT('',(-121.749401915016,150.,-102.999999999995));
#21910=CARTESIAN_POINT('',(-121.749401915016,118.3,-102.999999999995));
#21911=CARTESIAN_POINT('Origin',(-121.749401915016,150.,-90.5000000000001));
#21912=CARTESIAN_POINT('Origin',(-188.,118.3,-156.750598084983));
#21913=CARTESIAN_POINT('',(-188.,118.3,-169.250598084984));
#21914=CARTESIAN_POINT('Origin',(-188.,118.3,-156.750598084983));
#21915=CARTESIAN_POINT('',(-188.,150.,-169.250598084984));
#21916=CARTESIAN_POINT('',(-188.,118.3,-169.250598084984));
#21917=CARTESIAN_POINT('Origin',(-188.,150.,-156.750598084983));
#21918=CARTESIAN_POINT('Origin',(-278.5,118.3,-181.));
#21919=CARTESIAN_POINT('',(-278.5,118.3,-193.5));
#21920=CARTESIAN_POINT('Origin',(-278.5,118.3,-181.));
#21921=CARTESIAN_POINT('',(-278.5,150.,-193.5));
#21922=CARTESIAN_POINT('',(-278.5,118.3,-193.5));
#21923=CARTESIAN_POINT('Origin',(-278.5,150.,-181.));
#21924=CARTESIAN_POINT('Origin',(-278.5,118.3,-1.90240909456746E-14));
#21925=CARTESIAN_POINT('',(-278.5,118.3,-138.));
#21926=CARTESIAN_POINT('Origin',(-278.5,118.3,-1.90240909456746E-14));
#21927=CARTESIAN_POINT('',(-278.5,150.,-138.));
#21928=CARTESIAN_POINT('',(-278.5,118.3,-138.));
#21929=CARTESIAN_POINT('Origin',(-278.5,150.,-2.41218397451495E-14));
#21930=CARTESIAN_POINT('Origin',(-278.5,118.3,-1.90240909456746E-14));
#21931=CARTESIAN_POINT('',(-278.5,150.,-203.));
#21932=CARTESIAN_POINT('Origin',(-278.5,150.,-2.41218397451495E-14));
#21933=CARTESIAN_POINT('',(-278.5,118.3,-203.));
#21934=CARTESIAN_POINT('',(-278.5,118.3,-203.));
#21935=CARTESIAN_POINT('Origin',(-278.5,118.3,-1.90240909456746E-14));
#21936=CARTESIAN_POINT('Origin',(-278.5,118.3,-1.90240909456746E-14));
#21937=CARTESIAN_POINT('Origin',(-278.5,150.,-2.41218397451495E-14));
#21938=CARTESIAN_POINT('Origin',(-338.999999999999,210.25,-300.));
#21939=CARTESIAN_POINT('',(-329.499999999999,210.25,-300.));
#21940=CARTESIAN_POINT('Origin',(-338.999999999999,210.25,-300.));
#21941=CARTESIAN_POINT('',(-329.499999999999,242.,-300.));
#21942=CARTESIAN_POINT('',(-329.499999999999,210.25,-300.));
#21943=CARTESIAN_POINT('Origin',(-338.999999999999,242.,-300.));
#21944=CARTESIAN_POINT('Origin',(-278.499999999999,210.25,-239.5));
#21945=CARTESIAN_POINT('',(-268.999999999999,210.25,-239.5));
#21946=CARTESIAN_POINT('Origin',(-278.499999999999,210.25,-239.5));
#21947=CARTESIAN_POINT('',(-268.999999999999,242.,-239.5));
#21948=CARTESIAN_POINT('',(-268.999999999999,210.25,-239.5));
#21949=CARTESIAN_POINT('Origin',(-278.499999999999,242.,-239.5));
#21950=CARTESIAN_POINT('Origin',(-217.999999999999,210.25,-300.000000000001));
#21951=CARTESIAN_POINT('',(-208.499999999999,210.25,-300.000000000001));
#21952=CARTESIAN_POINT('Origin',(-217.999999999999,210.25,-300.000000000001));
#21953=CARTESIAN_POINT('',(-208.499999999999,242.,-300.000000000001));
#21954=CARTESIAN_POINT('',(-208.499999999999,210.25,-300.000000000001));
#21955=CARTESIAN_POINT('Origin',(-217.999999999999,242.,-300.000000000001));
#21956=CARTESIAN_POINT('Origin',(-278.5,210.25,-360.5));
#21957=CARTESIAN_POINT('',(-269.,210.25,-360.5));
#21958=CARTESIAN_POINT('Origin',(-278.5,210.25,-360.5));
#21959=CARTESIAN_POINT('',(-269.,242.,-360.5));
#21960=CARTESIAN_POINT('',(-269.,210.25,-360.5));
#21961=CARTESIAN_POINT('Origin',(-278.5,242.,-360.5));
#21962=CARTESIAN_POINT('Origin',(-278.5,210.25,-300.));
#21963=CARTESIAN_POINT('',(-247.5,210.25,-300.));
#21964=CARTESIAN_POINT('Origin',(-278.5,210.25,-300.));
#21965=CARTESIAN_POINT('',(-247.5,242.,-300.));
#21966=CARTESIAN_POINT('',(-247.5,210.25,-300.));
#21967=CARTESIAN_POINT('Origin',(-278.5,242.,-300.));
#21968=CARTESIAN_POINT('Origin',(-278.5,210.25,-300.));
#21969=CARTESIAN_POINT('',(-202.5,242.,-300.));
#21970=CARTESIAN_POINT('Origin',(-278.5,242.,-300.));
#21971=CARTESIAN_POINT('',(-202.5,210.25,-300.));
#21972=CARTESIAN_POINT('',(-202.5,210.25,-300.));
#21973=CARTESIAN_POINT('Origin',(-278.5,210.25,-300.));
#21974=CARTESIAN_POINT('Origin',(-278.5,210.25,-300.));
#21975=CARTESIAN_POINT('Origin',(-278.5,242.,-300.));
#21976=CARTESIAN_POINT('',(0.,0.,0.));
#21977=CARTESIAN_POINT('',(0.,0.,0.));
#21978=CARTESIAN_POINT('Origin',(-250.,0.,-200.));
#21979=CARTESIAN_POINT('',(-313.2,1.11022302462516E-13,-263.2));
#21980=CARTESIAN_POINT('',(-313.2,-0.199999999999922,-263.2));
#21981=CARTESIAN_POINT('',(-313.2,-3.33066907387547E-13,-263.2));
#21982=CARTESIAN_POINT('',(-250.,0.,-200.));
#21983=CARTESIAN_POINT('',(-281.6,1.11022302462516E-13,-231.6));
#21984=CARTESIAN_POINT('',(-250.,-63.2,-199.999999999999));
#21985=CARTESIAN_POINT('',(-250.,0.,-200.));
#21986=CARTESIAN_POINT('',(-250.2,-63.2,-200.2));
#21987=CARTESIAN_POINT('',(-250.,-63.2,-200.));
#21988=CARTESIAN_POINT('',(-257.9375,-55.4625,-207.937499999999));
#21989=CARTESIAN_POINT('Origin',(-250.199999999997,-55.4624999999972,-200.199999999997));
#21990=CARTESIAN_POINT('',(-257.9375,-15.875,-207.9375));
#21991=CARTESIAN_POINT('',(-257.9375,-55.4625000000001,-207.937499999999));
#21992=CARTESIAN_POINT('',(-265.875,-7.93749999999999,-215.875));
#21993=CARTESIAN_POINT('Origin',(-265.875000000001,-15.875000000001,-215.875000000001));
#21994=CARTESIAN_POINT('',(-305.4625,-7.93749999999988,-255.4625));
#21995=CARTESIAN_POINT('',(-257.9375,-7.93749999999999,-207.9375));
#21996=CARTESIAN_POINT('Origin',(-305.462499999999,-0.199999999998104,-255.462499999999));
#21997=CARTESIAN_POINT('Origin',(-250.,0.,200.));
#21998=CARTESIAN_POINT('',(-313.2,0.,263.2));
#21999=CARTESIAN_POINT('',(-250.,0.,200.));
#22000=CARTESIAN_POINT('',(-81.5999999999998,0.,31.5999999999999));
#22001=CARTESIAN_POINT('',(-313.2,-0.199999999999978,263.2));
#22002=CARTESIAN_POINT('',(-313.2,9.71445146547012E-12,263.2));
#22003=CARTESIAN_POINT('',(-305.4625,-7.93749999999999,255.4625));
#22004=CARTESIAN_POINT('Origin',(-305.462500000002,-0.200000000002175,255.462500000002));
#22005=CARTESIAN_POINT('',(-265.875,-7.93749999999999,215.875));
#22006=CARTESIAN_POINT('',(-57.9374999999998,-7.93749999999999,7.93749999999999));
#22007=CARTESIAN_POINT('',(-257.9375,-15.875,207.9375));
#22008=CARTESIAN_POINT('Origin',(-265.875000000001,-15.8750000000013,215.875000000002));
#22009=CARTESIAN_POINT('',(-257.9375,-55.4625,207.937500000001));
#22010=CARTESIAN_POINT('',(-257.9375,-55.4624999999943,207.937500000001));
#22011=CARTESIAN_POINT('',(-250.2,-63.2,200.200000000001));
#22012=CARTESIAN_POINT('Origin',(-250.2,-55.4625000000004,200.200000000001));
#22013=CARTESIAN_POINT('',(-250.,-63.2,200.000000000001));
#22014=CARTESIAN_POINT('',(-49.9999999999996,-63.2000000000014,5.55111512312578E-13));
#22015=CARTESIAN_POINT('',(-250.,5.55111512312578E-12,200.));
#22016=CARTESIAN_POINT('Origin',(-313.2,0.,-200.));
#22017=CARTESIAN_POINT('',(-250.,0.,-200.));
#22018=CARTESIAN_POINT('',(-313.2,0.,-200.));
#22019=CARTESIAN_POINT('Origin',(-250.,0.,-200.));
#22020=CARTESIAN_POINT('',(-250.,-63.2,-200.));
#22021=CARTESIAN_POINT('Origin',(-250.,-63.2,-200.));
#22022=CARTESIAN_POINT('',(-250.2,-63.2,-200.));
#22023=CARTESIAN_POINT('Origin',(-250.2,-55.4625,-200.));
#22024=CARTESIAN_POINT('',(-257.9375,-55.4625,-200.));
#22025=CARTESIAN_POINT('Origin',(-257.9375,-55.4625,-200.));
#22026=CARTESIAN_POINT('',(-257.9375,-15.875,-200.));
#22027=CARTESIAN_POINT('Origin',(-265.875,-15.875,-200.));
#22028=CARTESIAN_POINT('',(-265.875,-7.93749999999999,-200.));
#22029=CARTESIAN_POINT('Origin',(-265.875,-7.93749999999999,-200.));
#22030=CARTESIAN_POINT('',(-305.4625,-7.93749999999999,-200.));
#22031=CARTESIAN_POINT('Origin',(-305.4625,-0.199999999999978,-200.));
#22032=CARTESIAN_POINT('',(-313.2,-0.199999999999978,-200.));
#22033=CARTESIAN_POINT('Origin',(-313.2,0.,-200.));
#22034=CARTESIAN_POINT('Origin',(-250.,0.,-200.));
#22035=CARTESIAN_POINT('',(-313.2,-0.199999999999922,-263.2));
#22036=CARTESIAN_POINT('',(-313.2,1.11022302462516E-13,-263.2));
#22037=CARTESIAN_POINT('',(-313.2,1.18793863634892E-11,-263.2));
#22038=CARTESIAN_POINT('',(-305.4625,-7.93749999999988,-255.4625));
#22039=CARTESIAN_POINT('Origin',(-305.4625,-0.19999999999989,-255.4625));
#22040=CARTESIAN_POINT('',(-265.875,-7.93749999999999,-215.875));
#22041=CARTESIAN_POINT('',(-7.93749999999999,-7.93749999999999,42.0625000000001));
#22042=CARTESIAN_POINT('',(-257.9375,-15.875,-207.9375));
#22043=CARTESIAN_POINT('Origin',(-265.875000000001,-15.8750000000005,-215.875000000001));
#22044=CARTESIAN_POINT('',(-257.937500000001,-55.4625,-207.9375));
#22045=CARTESIAN_POINT('',(-257.937500000001,-55.4624999999929,-207.9375));
#22046=CARTESIAN_POINT('',(-250.200000000001,-63.2,-200.2));
#22047=CARTESIAN_POINT('Origin',(-250.200000000001,-55.4624999999997,-200.2));
#22048=CARTESIAN_POINT('',(-250.000000000001,-63.2,-200.));
#22049=CARTESIAN_POINT('',(-4.99600519899998E-13,-63.2000000000018,50.0000000000003));
#22050=CARTESIAN_POINT('',(-250.,0.,-200.));
#22051=CARTESIAN_POINT('',(-250.,6.93889390390723E-12,-200.));
#22052=CARTESIAN_POINT('',(-31.5999999999999,0.,18.4000000000001));
#22053=CARTESIAN_POINT('Origin',(250.,0.,-200.));
#22054=CARTESIAN_POINT('',(250.,0.,-200.));
#22055=CARTESIAN_POINT('',(313.2,1.11022302462516E-13,-263.2));
#22056=CARTESIAN_POINT('',(281.6,1.11022302462516E-13,-231.6));
#22057=CARTESIAN_POINT('',(250.,-63.2,-200.));
#22058=CARTESIAN_POINT('',(250.,0.,-200.));
#22059=CARTESIAN_POINT('',(250.2,-63.2,-200.2));
#22060=CARTESIAN_POINT('',(250.,-63.2,-200.));
#22061=CARTESIAN_POINT('',(257.9375,-55.4625,-207.9375));
#22062=CARTESIAN_POINT('Origin',(250.200000000001,-55.4625000000011,-200.200000000001));
#22063=CARTESIAN_POINT('',(257.9375,-15.875,-207.9375));
#22064=CARTESIAN_POINT('',(257.9375,-55.4625000000001,-207.9375));
#22065=CARTESIAN_POINT('',(265.875,-7.93749999999999,-215.875));
#22066=CARTESIAN_POINT('Origin',(265.874999999997,-15.8749999999967,-215.874999999997));
#22067=CARTESIAN_POINT('',(305.4625,-7.93749999999988,-255.4625));
#22068=CARTESIAN_POINT('',(257.9375,-7.93749999999999,-207.9375));
#22069=CARTESIAN_POINT('',(313.2,-0.199999999999867,-263.2));
#22070=CARTESIAN_POINT('Origin',(305.4625,-0.199999999999467,-255.4625));
#22071=CARTESIAN_POINT('',(313.2,1.11022302462516E-13,-263.2));
#22072=CARTESIAN_POINT('Origin',(250.,1.11022302462516E-13,-263.2));
#22073=CARTESIAN_POINT('',(250.,1.11022302462516E-13,-263.2));
#22074=CARTESIAN_POINT('',(250.,0.,-200.));
#22075=CARTESIAN_POINT('Origin',(250.,0.,-200.));
#22076=CARTESIAN_POINT('',(250.,-63.2,-200.));
#22077=CARTESIAN_POINT('Origin',(250.,-63.2,-200.));
#22078=CARTESIAN_POINT('',(250.,-63.2,-200.2));
#22079=CARTESIAN_POINT('Origin',(250.,-55.4625,-200.2));
#22080=CARTESIAN_POINT('',(250.,-55.4625,-207.9375));
#22081=CARTESIAN_POINT('Origin',(250.,-55.4625,-207.9375));
#22082=CARTESIAN_POINT('',(250.,-15.875,-207.9375));
#22083=CARTESIAN_POINT('Origin',(250.,-15.875,-215.875));
#22084=CARTESIAN_POINT('',(250.,-7.93749999999999,-215.875));
#22085=CARTESIAN_POINT('Origin',(250.,-7.93749999999999,-215.875));
#22086=CARTESIAN_POINT('',(250.,-7.93749999999993,-255.4625));
#22087=CARTESIAN_POINT('Origin',(250.,-0.199999999999922,-255.4625));
#22088=CARTESIAN_POINT('',(250.,-0.199999999999922,-263.2));
#22089=CARTESIAN_POINT('Origin',(250.,1.11022302462516E-13,-263.2));
#22090=CARTESIAN_POINT('Origin',(250.,0.,200.));
#22091=CARTESIAN_POINT('',(313.2,-0.199999999999978,263.2));
#22092=CARTESIAN_POINT('',(313.2,0.,263.2));
#22093=CARTESIAN_POINT('',(313.2,7.88258347483861E-12,263.2));
#22094=CARTESIAN_POINT('',(305.4625,-7.93749999999999,255.4625));
#22095=CARTESIAN_POINT('Origin',(305.462500000003,-0.200000000002943,255.462500000003));
#22096=CARTESIAN_POINT('',(265.875,-7.93749999999999,215.875));
#22097=CARTESIAN_POINT('',(7.93749999999993,-7.93749999999988,-42.0625));
#22098=CARTESIAN_POINT('',(257.9375,-15.875,207.9375));
#22099=CARTESIAN_POINT('Origin',(265.874999999999,-15.8749999999993,215.874999999999));
#22100=CARTESIAN_POINT('',(257.9375,-55.4625,207.9375));
#22101=CARTESIAN_POINT('',(257.9375,-55.4624999999965,207.9375));
#22102=CARTESIAN_POINT('',(250.2,-63.2,200.2));
#22103=CARTESIAN_POINT('Origin',(250.200000000001,-55.4625000000004,200.200000000001));
#22104=CARTESIAN_POINT('',(250.,-63.2,200.));
#22105=CARTESIAN_POINT('',(3.88578111558364E-13,-63.2000000000016,-50.));
#22106=CARTESIAN_POINT('',(250.,0.,200.));
#22107=CARTESIAN_POINT('',(250.,3.49720252756924E-12,200.));
#22108=CARTESIAN_POINT('',(31.5999999999999,5.55111512312578E-14,-18.4));
#22109=CARTESIAN_POINT('Origin',(-250.,0.,200.));
#22110=CARTESIAN_POINT('',(-250.,0.,200.));
#22111=CARTESIAN_POINT('',(-313.2,0.,263.2));
#22112=CARTESIAN_POINT('',(-281.6,0.,231.6));
#22113=CARTESIAN_POINT('',(-250.,-63.2,200.));
#22114=CARTESIAN_POINT('',(-250.,0.,200.));
#22115=CARTESIAN_POINT('',(-250.199999999999,-63.2,200.2));
#22116=CARTESIAN_POINT('',(-250.,-63.2,200.));
#22117=CARTESIAN_POINT('',(-257.937499999999,-55.4625,207.9375));
#22118=CARTESIAN_POINT('Origin',(-250.199999999999,-55.4624999999993,200.2));
#22119=CARTESIAN_POINT('',(-257.9375,-15.875,207.9375));
#22120=CARTESIAN_POINT('',(-257.937499999999,-55.4625000000001,207.9375));
#22121=CARTESIAN_POINT('',(-265.875,-7.93749999999999,215.875));
#22122=CARTESIAN_POINT('Origin',(-265.874999999999,-15.8749999999987,215.874999999999));
#22123=CARTESIAN_POINT('',(-305.4625,-7.93749999999999,255.4625));
#22124=CARTESIAN_POINT('',(-257.9375,-7.93749999999999,207.9375));
#22125=CARTESIAN_POINT('',(-313.2,-0.199999999999978,263.2));
#22126=CARTESIAN_POINT('Origin',(-305.462499999999,-0.199999999999151,255.462499999999));
#22127=CARTESIAN_POINT('',(-313.2,-4.44089209850063E-13,263.2));
#22128=CARTESIAN_POINT('Origin',(-250.,0.,263.2));
#22129=CARTESIAN_POINT('',(-250.,0.,263.2));
#22130=CARTESIAN_POINT('',(-250.,0.,200.));
#22131=CARTESIAN_POINT('Origin',(-250.,0.,200.));
#22132=CARTESIAN_POINT('',(-250.,-63.2,200.));
#22133=CARTESIAN_POINT('Origin',(-250.,-63.2,200.));
#22134=CARTESIAN_POINT('',(-250.,-63.2,200.2));
#22135=CARTESIAN_POINT('Origin',(-250.,-55.4625,200.2));
#22136=CARTESIAN_POINT('',(-250.,-55.4625,207.9375));
#22137=CARTESIAN_POINT('Origin',(-250.,-55.4625,207.9375));
#22138=CARTESIAN_POINT('',(-250.,-15.875,207.9375));
#22139=CARTESIAN_POINT('Origin',(-250.,-15.875,215.875));
#22140=CARTESIAN_POINT('',(-250.,-7.93749999999999,215.875));
#22141=CARTESIAN_POINT('Origin',(-250.,-7.93749999999999,215.875));
#22142=CARTESIAN_POINT('',(-250.,-7.93749999999999,255.4625));
#22143=CARTESIAN_POINT('Origin',(-250.,-0.199999999999978,255.4625));
#22144=CARTESIAN_POINT('',(-250.,-0.199999999999978,263.2));
#22145=CARTESIAN_POINT('Origin',(-250.,0.,263.2));
#22146=CARTESIAN_POINT('Origin',(-340.039729762984,1.11022302462516E-13,
155.0625));
#22147=CARTESIAN_POINT('',(-349.039729762984,1.09920120343283E-13,155.0625));
#22148=CARTESIAN_POINT('Origin',(-340.039729762984,1.11022302462516E-13,
155.0625));
#22149=CARTESIAN_POINT('',(-349.039729762984,1.09920120343283E-13,163.));
#22150=CARTESIAN_POINT('',(-349.039729762984,1.09920120343283E-13,155.0625));
#22151=CARTESIAN_POINT('Origin',(-340.039729762984,0.,163.));
#22152=CARTESIAN_POINT('Origin',(-340.039729762984,1.11022302462516E-13,
155.0625));
#22153=CARTESIAN_POINT('',(-318.170320326478,-2.39351851851843,155.0625));
#22154=CARTESIAN_POINT('',(-340.039729762984,-21.9999999999999,155.0625));
#22155=CARTESIAN_POINT('Origin',(-340.039729762984,1.11022302462516E-13,
155.0625));
#22156=CARTESIAN_POINT('',(-340.039729762984,-22.,163.));
#22157=CARTESIAN_POINT('',(-340.039729762984,-21.9999999999999,155.0625));
#22158=CARTESIAN_POINT('',(-318.170320326478,-2.39351851851854,163.));
#22159=CARTESIAN_POINT('Origin',(-340.039729762984,0.,163.));
#22160=CARTESIAN_POINT('',(-318.170320326478,-2.39351851851843,155.0625));
#22161=CARTESIAN_POINT('Origin',(-313.2,-2.93749999999993,155.0625));
#22162=CARTESIAN_POINT('',(-313.2,-7.93749999999999,163.));
#22163=CARTESIAN_POINT('Origin',(-313.2,-2.93749999999998,163.));
#22164=CARTESIAN_POINT('',(-313.2,-7.93749999999988,155.0625));
#22165=CARTESIAN_POINT('',(-313.2,-7.93749999999988,155.0625));
#22166=CARTESIAN_POINT('Origin',(-313.2,-2.93749999999993,155.0625));
#22167=CARTESIAN_POINT('Origin',(-265.039729762984,-7.93749999999988,155.0625));
#22168=CARTESIAN_POINT('',(-265.039729762984,-7.93749999999999,163.));
#22169=CARTESIAN_POINT('',(-265.039729762984,-7.93749999999999,163.));
#22170=CARTESIAN_POINT('',(-265.039729762984,-7.93749999999988,155.0625));
#22171=CARTESIAN_POINT('',(-265.039729762984,-7.93749999999988,155.0625));
#22172=CARTESIAN_POINT('',(-265.039729762984,-7.93749999999988,155.0625));
#22173=CARTESIAN_POINT('Origin',(-260.039729762984,-12.9374999999999,155.0625));
#22174=CARTESIAN_POINT('',(-260.039729762984,-12.9375,163.));
#22175=CARTESIAN_POINT('',(-260.039729762984,-12.9375,163.));
#22176=CARTESIAN_POINT('',(-260.039729762984,-12.9374999999999,155.0625));
#22177=CARTESIAN_POINT('',(-260.039729762984,-12.9374999999999,155.0625));
#22178=CARTESIAN_POINT('',(-260.039729762984,-12.9374999999999,155.0625));
#22179=CARTESIAN_POINT('Origin',(-260.039729762984,-21.9999999999999,155.0625));
#22180=CARTESIAN_POINT('',(-260.039729762984,-22.,163.));
#22181=CARTESIAN_POINT('',(-260.039729762984,-22.,163.));
#22182=CARTESIAN_POINT('',(-260.039729762984,-21.9999999999999,155.0625));
#22183=CARTESIAN_POINT('',(-260.039729762984,-21.9999999999999,155.0625));
#22184=CARTESIAN_POINT('',(-260.039729762984,-21.9999999999999,155.0625));
#22185=CARTESIAN_POINT('Origin',(-340.039729762984,-21.9999999999999,155.0625));
#22186=CARTESIAN_POINT('',(-340.039729762984,-22.,163.));
#22187=CARTESIAN_POINT('',(-340.039729762984,-21.9999999999999,155.0625));
#22188=CARTESIAN_POINT('Origin',(-340.039729762984,1.11022302462516E-13,
155.0625));
#22189=CARTESIAN_POINT('Origin',(-340.039729762984,0.,163.));
#22190=CARTESIAN_POINT('Origin',(286.9375,-36.9375,178.55));
#22191=CARTESIAN_POINT('',(295.9375,-36.9375,178.55));
#22192=CARTESIAN_POINT('Origin',(286.9375,-36.9375,178.55));
#22193=CARTESIAN_POINT('',(295.9375,-36.9375,172.2));
#22194=CARTESIAN_POINT('',(295.9375,-36.9375,178.55));
#22195=CARTESIAN_POINT('Origin',(286.9375,-36.9375,172.2));
#22196=CARTESIAN_POINT('Origin',(286.9375,-36.9375,178.55));
#22197=CARTESIAN_POINT('',(265.875,-7.93749999999999,178.55));
#22198=CARTESIAN_POINT('',(257.9375,-15.874999999997,178.55));
#22199=CARTESIAN_POINT('',(257.9375,-15.874999999997,178.55));
#22200=CARTESIAN_POINT('',(257.9375,-55.9375,178.55));
#22201=CARTESIAN_POINT('',(257.9375,-55.9375,178.55));
#22202=CARTESIAN_POINT('',(286.9375,-55.9375,178.55));
#22203=CARTESIAN_POINT('',(286.9375,-55.9375,178.55));
#22204=CARTESIAN_POINT('',(305.9375,-36.9375,178.55));
#22205=CARTESIAN_POINT('Origin',(286.9375,-36.9375,178.55));
#22206=CARTESIAN_POINT('',(305.9375,-7.93749999999999,178.55));
#22207=CARTESIAN_POINT('',(305.9375,-7.93749999999999,178.55));
#22208=CARTESIAN_POINT('',(265.875,-7.93749999999999,178.55));
#22209=CARTESIAN_POINT('Origin',(286.9375,-36.9375,172.2));
#22210=CARTESIAN_POINT('',(265.875,-7.93749999999999,172.2));
#22211=CARTESIAN_POINT('',(257.9375,-15.874999999997,172.2));
#22212=CARTESIAN_POINT('',(257.9375,-15.874999999997,172.2));
#22213=CARTESIAN_POINT('',(305.9375,-7.93749999999999,172.2));
#22214=CARTESIAN_POINT('',(265.875,-7.93749999999999,172.2));
#22215=CARTESIAN_POINT('',(305.9375,-36.9375,172.2));
#22216=CARTESIAN_POINT('',(305.9375,-7.93749999999999,172.2));
#22217=CARTESIAN_POINT('',(286.9375,-55.9375,172.2));
#22218=CARTESIAN_POINT('Origin',(286.9375,-36.9375,172.2));
#22219=CARTESIAN_POINT('',(257.9375,-55.9375,172.2));
#22220=CARTESIAN_POINT('',(286.9375,-55.9375,172.2));
#22221=CARTESIAN_POINT('',(257.9375,-55.9375,172.2));
#22222=CARTESIAN_POINT('Origin',(257.9375,-15.874999999997,178.55));
#22223=CARTESIAN_POINT('',(257.9375,-15.874999999997,178.55));
#22224=CARTESIAN_POINT('',(265.875,-7.93749999999999,178.55));
#22225=CARTESIAN_POINT('Origin',(257.9375,-55.9375,178.55));
#22226=CARTESIAN_POINT('',(257.9375,-55.9375,178.55));
#22227=CARTESIAN_POINT('Origin',(286.9375,-55.9375,178.55));
#22228=CARTESIAN_POINT('',(286.9375,-55.9375,178.55));
#22229=CARTESIAN_POINT('Origin',(286.9375,-36.9375,178.55));
#22230=CARTESIAN_POINT('',(305.9375,-36.9375,178.55));
#22231=CARTESIAN_POINT('Origin',(305.9375,-7.93749999999999,178.55));
#22232=CARTESIAN_POINT('',(305.9375,-7.93749999999999,178.55));
#22233=CARTESIAN_POINT('Origin',(265.875,-7.93749999999999,178.55));
#22234=CARTESIAN_POINT('Origin',(-340.039729762984,0.,-155.0625));
#22235=CARTESIAN_POINT('',(-349.039729762984,1.10218211923262E-15,-155.0625));
#22236=CARTESIAN_POINT('Origin',(-340.039729762984,0.,-155.0625));
#22237=CARTESIAN_POINT('',(-349.039729762984,1.10218211923262E-15,-163.));
#22238=CARTESIAN_POINT('',(-349.039729762984,1.10218211923262E-15,-155.0625));
#22239=CARTESIAN_POINT('Origin',(-340.039729762984,0.,-163.));
#22240=CARTESIAN_POINT('Origin',(-340.039729762984,0.,-155.0625));
#22241=CARTESIAN_POINT('',(-318.170320326478,-2.39351851851849,-155.0625));
#22242=CARTESIAN_POINT('',(-340.039729762984,-22.,-155.0625));
#22243=CARTESIAN_POINT('Origin',(-340.039729762984,0.,-155.0625));
#22244=CARTESIAN_POINT('',(-318.170320326478,-2.39351851851849,-163.));
#22245=CARTESIAN_POINT('',(-318.170320326478,-2.39351851851849,-155.0625));
#22246=CARTESIAN_POINT('',(-340.039729762984,-22.,-163.));
#22247=CARTESIAN_POINT('Origin',(-340.039729762984,0.,-163.));
#22248=CARTESIAN_POINT('',(-340.039729762984,-22.,-155.0625));
#22249=CARTESIAN_POINT('Origin',(-313.2,-2.93749999999998,-155.0625));
#22250=CARTESIAN_POINT('',(-313.2,-7.93749999999999,-163.));
#22251=CARTESIAN_POINT('Origin',(-313.2,-2.93749999999998,-163.));
#22252=CARTESIAN_POINT('',(-313.2,-7.93749999999999,-155.0625));
#22253=CARTESIAN_POINT('Origin',(-313.2,-2.93749999999998,-155.0625));
#22254=CARTESIAN_POINT('',(-313.2,-7.93749999999999,-155.0625));
#22255=CARTESIAN_POINT('Origin',(-265.039729762984,-7.93749999999999,-155.0625));
#22256=CARTESIAN_POINT('',(-265.039729762984,-7.93749999999999,-163.));
#22257=CARTESIAN_POINT('',(-265.039729762984,-7.93749999999999,-163.));
#22258=CARTESIAN_POINT('',(-265.039729762984,-7.93749999999999,-155.0625));
#22259=CARTESIAN_POINT('',(-265.039729762984,-7.93749999999999,-155.0625));
#22260=CARTESIAN_POINT('',(-265.039729762984,-7.93749999999999,-155.0625));
#22261=CARTESIAN_POINT('Origin',(-260.039729762984,-12.9374999999999,-155.0625));
#22262=CARTESIAN_POINT('',(-260.039729762984,-12.9374999999999,-163.));
#22263=CARTESIAN_POINT('',(-260.039729762984,-12.9374999999999,-163.));
#22264=CARTESIAN_POINT('',(-260.039729762984,-12.9374999999999,-155.0625));
#22265=CARTESIAN_POINT('',(-260.039729762984,-12.9374999999999,-155.0625));
#22266=CARTESIAN_POINT('',(-260.039729762984,-12.9374999999999,-155.0625));
#22267=CARTESIAN_POINT('Origin',(-260.039729762984,-22.,-155.0625));
#22268=CARTESIAN_POINT('',(-260.039729762984,-22.,-163.));
#22269=CARTESIAN_POINT('',(-260.039729762984,-22.,-163.));
#22270=CARTESIAN_POINT('',(-260.039729762984,-22.,-155.0625));
#22271=CARTESIAN_POINT('',(-260.039729762984,-22.,-155.0625));
#22272=CARTESIAN_POINT('',(-260.039729762984,-22.,-155.0625));
#22273=CARTESIAN_POINT('Origin',(-340.039729762984,-22.,-155.0625));
#22274=CARTESIAN_POINT('',(-340.039729762984,-22.,-163.));
#22275=CARTESIAN_POINT('',(-340.039729762984,-22.,-155.0625));
#22276=CARTESIAN_POINT('Origin',(-340.039729762984,0.,-155.0625));
#22277=CARTESIAN_POINT('Origin',(-340.039729762984,0.,-163.));
#22278=CARTESIAN_POINT('Origin',(286.9375,-36.9375,-178.55));
#22279=CARTESIAN_POINT('',(295.9375,-36.9375,-178.55));
#22280=CARTESIAN_POINT('Origin',(286.9375,-36.9375,-178.55));
#22281=CARTESIAN_POINT('',(295.9375,-36.9375,-172.2));
#22282=CARTESIAN_POINT('',(295.9375,-36.9375,-178.55));
#22283=CARTESIAN_POINT('Origin',(286.9375,-36.9375,-172.2));
#22284=CARTESIAN_POINT('Origin',(286.9375,-36.9375,-178.55));
#22285=CARTESIAN_POINT('',(265.875,-7.93749999999999,-178.55));
#22286=CARTESIAN_POINT('',(257.9375,-15.874999999997,-178.55));
#22287=CARTESIAN_POINT('',(257.9375,-15.874999999997,-178.55));
#22288=CARTESIAN_POINT('',(305.9375,-7.93749999999999,-178.55));
#22289=CARTESIAN_POINT('',(265.875,-7.93749999999999,-178.55));
#22290=CARTESIAN_POINT('',(305.9375,-36.9375,-178.55));
#22291=CARTESIAN_POINT('',(305.9375,-7.93749999999999,-178.55));
#22292=CARTESIAN_POINT('',(286.9375,-55.9375,-178.55));
#22293=CARTESIAN_POINT('Origin',(286.9375,-36.9375,-178.55));
#22294=CARTESIAN_POINT('',(257.9375,-55.9375,-178.55));
#22295=CARTESIAN_POINT('',(286.9375,-55.9375,-178.55));
#22296=CARTESIAN_POINT('',(257.9375,-55.9375,-178.55));
#22297=CARTESIAN_POINT('Origin',(286.9375,-36.9375,-172.2));
#22298=CARTESIAN_POINT('',(265.875,-7.93749999999999,-172.2));
#22299=CARTESIAN_POINT('',(257.9375,-15.874999999997,-172.2));
#22300=CARTESIAN_POINT('',(257.9375,-15.874999999997,-172.2));
#22301=CARTESIAN_POINT('',(257.9375,-55.9375,-172.2));
#22302=CARTESIAN_POINT('',(257.9375,-55.9375,-172.2));
#22303=CARTESIAN_POINT('',(286.9375,-55.9375,-172.2));
#22304=CARTESIAN_POINT('',(286.9375,-55.9375,-172.2));
#22305=CARTESIAN_POINT('',(305.9375,-36.9375,-172.2));
#22306=CARTESIAN_POINT('Origin',(286.9375,-36.9375,-172.2));
#22307=CARTESIAN_POINT('',(305.9375,-7.93749999999999,-172.2));
#22308=CARTESIAN_POINT('',(305.9375,-7.93749999999999,-172.2));
#22309=CARTESIAN_POINT('',(265.875,-7.93749999999999,-172.2));
#22310=CARTESIAN_POINT('Origin',(257.9375,-15.874999999997,-178.55));
#22311=CARTESIAN_POINT('',(265.875,-7.93749999999999,-178.55));
#22312=CARTESIAN_POINT('',(257.9375,-15.874999999997,-178.55));
#22313=CARTESIAN_POINT('Origin',(257.9375,-55.9375,-178.55));
#22314=CARTESIAN_POINT('',(257.9375,-55.9375,-178.55));
#22315=CARTESIAN_POINT('Origin',(286.9375,-55.9375,-178.55));
#22316=CARTESIAN_POINT('',(286.9375,-55.9375,-178.55));
#22317=CARTESIAN_POINT('Origin',(286.9375,-36.9375,-178.55));
#22318=CARTESIAN_POINT('',(305.9375,-36.9375,-178.55));
#22319=CARTESIAN_POINT('Origin',(305.9375,-7.93749999999999,-178.55));
#22320=CARTESIAN_POINT('',(305.9375,-7.93749999999999,-178.55));
#22321=CARTESIAN_POINT('Origin',(265.875,-7.93749999999999,-178.55));
#22322=CARTESIAN_POINT('Origin',(284.2,-10.000000000002,-163.2));
#22323=CARTESIAN_POINT('',(284.2,-7.93749999999716,-154.2));
#22324=CARTESIAN_POINT('',(284.2,-7.93749999999716,-172.2));
#22325=CARTESIAN_POINT('Origin',(284.2,-7.9374999999971,-163.2));
#22326=CARTESIAN_POINT('',(284.2,-1.99840144432528E-12,-172.2));
#22327=CARTESIAN_POINT('',(284.2,-10.000000000002,-172.2));
#22328=CARTESIAN_POINT('',(284.2,-1.99840144432528E-12,-154.2));
#22329=CARTESIAN_POINT('Origin',(284.2,-1.99840144432528E-12,-163.2));
#22330=CARTESIAN_POINT('',(284.2,-10.000000000002,-154.2));
#22331=CARTESIAN_POINT('Origin',(284.2,-10.000000000002,163.2));
#22332=CARTESIAN_POINT('',(284.2,-7.93749999999716,172.2));
#22333=CARTESIAN_POINT('',(284.2,-7.93749999999704,154.2));
#22334=CARTESIAN_POINT('Origin',(284.2,-7.9374999999971,163.2));
#22335=CARTESIAN_POINT('',(284.2,-1.88737914186277E-12,154.2));
#22336=CARTESIAN_POINT('',(284.2,-10.0000000000019,154.2));
#22337=CARTESIAN_POINT('',(284.2,-1.99840144432528E-12,172.2));
#22338=CARTESIAN_POINT('Origin',(284.2,-1.99840144432528E-12,163.2));
#22339=CARTESIAN_POINT('',(284.2,-10.000000000002,172.2));
#22340=CARTESIAN_POINT('Origin',(305.4625,-0.199999999997258,200.));
#22341=CARTESIAN_POINT('',(313.2,-0.199999999997258,-154.2));
#22342=CARTESIAN_POINT('',(305.4625,-7.93749999999721,-154.2));
#22343=CARTESIAN_POINT('Origin',(305.4625,-0.199999999997202,-154.2));
#22344=CARTESIAN_POINT('',(313.2,-0.199999999997202,154.2));
#22345=CARTESIAN_POINT('',(313.2,-0.199999999997258,200.));
#22346=CARTESIAN_POINT('',(305.4625,-7.93749999999716,154.2));
#22347=CARTESIAN_POINT('Origin',(305.4625,-0.199999999997147,154.2));
#22348=CARTESIAN_POINT('',(305.4625,-7.93749999999721,200.));
#22349=CARTESIAN_POINT('Origin',(305.4625,-0.199999999997258,200.));
#22350=CARTESIAN_POINT('',(313.2,-0.199999999997313,172.2));
#22351=CARTESIAN_POINT('',(305.4625,-7.93749999999727,172.2));
#22352=CARTESIAN_POINT('Origin',(305.4625,-0.199999999997258,172.2));
#22353=CARTESIAN_POINT('',(313.2,-0.199999999997258,263.2));
#22354=CARTESIAN_POINT('',(313.2,-0.199999999997258,200.));
#22355=CARTESIAN_POINT('',(305.4625,-7.93749999999721,255.4625));
#22356=CARTESIAN_POINT('Origin',(305.462500000002,-0.199999999999014,255.462500000001));
#22357=CARTESIAN_POINT('',(305.4625,-7.93749999999721,200.));
#22358=CARTESIAN_POINT('Origin',(313.2,2.72004641033163E-12,200.));
#22359=CARTESIAN_POINT('',(313.2,-2.22044604925031E-12,-154.2));
#22360=CARTESIAN_POINT('',(313.2,2.72004641033163E-12,-154.2));
#22361=CARTESIAN_POINT('',(313.2,-2.1094237467878E-12,154.2));
#22362=CARTESIAN_POINT('',(313.2,2.72004641033163E-12,200.));
#22363=CARTESIAN_POINT('',(313.2,2.77555756156289E-12,154.2));
#22364=CARTESIAN_POINT('Origin',(313.2,2.72004641033163E-12,200.));
#22365=CARTESIAN_POINT('',(313.2,-2.22044604925031E-12,172.2));
#22366=CARTESIAN_POINT('',(313.2,2.72004641033163E-12,172.2));
#22367=CARTESIAN_POINT('',(313.2,2.72004641033163E-12,263.2));
#22368=CARTESIAN_POINT('',(313.2,2.72004641033163E-12,200.));
#22369=CARTESIAN_POINT('',(313.2,2.27595720048157E-12,263.2));
#22370=CARTESIAN_POINT('Origin',(250.,0.,-200.));
#22371=CARTESIAN_POINT('',(313.2,-0.199999999997202,-263.2));
#22372=CARTESIAN_POINT('',(313.2,2.77555756156289E-12,-263.2));
#22373=CARTESIAN_POINT('',(313.2,6.0507154842071E-12,-263.2));
#22374=CARTESIAN_POINT('',(305.4625,-7.93749999999716,-255.4625));
#22375=CARTESIAN_POINT('Origin',(305.462499999999,-0.199999999996119,-255.462499999999));
#22376=CARTESIAN_POINT('',(265.875,-7.93749999999699,-215.875));
#22377=CARTESIAN_POINT('',(57.9375,-7.93749999999554,-7.93749999999999));
#22378=CARTESIAN_POINT('',(257.9375,-15.8749999999969,-207.9375));
#22379=CARTESIAN_POINT('Origin',(265.875000000002,-15.8749999999988,-215.875000000002));
#22380=CARTESIAN_POINT('',(257.9375,-55.4624999999969,-207.9375));
#22381=CARTESIAN_POINT('',(257.9375,-55.4624999999969,-207.9375));
#22382=CARTESIAN_POINT('',(250.2,-63.1999999999969,-200.2));
#22383=CARTESIAN_POINT('Origin',(250.200000000003,-55.4625000000002,-200.200000000003));
#22384=CARTESIAN_POINT('',(250.,-63.1999999999969,-200.));
#22385=CARTESIAN_POINT('',(49.9999999999996,-63.1999999999969,0.));
#22386=CARTESIAN_POINT('',(250.,3.1641356201817E-12,-200.));
#22387=CARTESIAN_POINT('',(250.,3.10862446895044E-12,-200.));
#22388=CARTESIAN_POINT('',(81.6,4.32986979603811E-12,-31.6));
#22389=CARTESIAN_POINT('Origin',(250.,0.,200.));
#22390=CARTESIAN_POINT('',(250.,3.1641356201817E-12,200.));
#22391=CARTESIAN_POINT('',(281.6,2.94209101525666E-12,231.6));
#22392=CARTESIAN_POINT('',(250.,-63.1999999999969,200.));
#22393=CARTESIAN_POINT('',(250.,3.1641356201817E-12,200.));
#22394=CARTESIAN_POINT('',(250.2,-63.1999999999969,200.199999999999));
#22395=CARTESIAN_POINT('',(250.,-63.1999999999969,200.));
#22396=CARTESIAN_POINT('',(257.9375,-55.4624999999969,207.937499999999));
#22397=CARTESIAN_POINT('Origin',(250.200000000002,-55.4624999999997,200.200000000002));
#22398=CARTESIAN_POINT('',(257.9375,-15.8749999999969,207.9375));
#22399=CARTESIAN_POINT('',(257.9375,-55.462499999997,207.937499999999));
#22400=CARTESIAN_POINT('',(265.875,-7.93749999999693,215.875));
#22401=CARTESIAN_POINT('Origin',(265.875,-15.8749999999973,215.875));
#22402=CARTESIAN_POINT('',(257.9375,-7.93749999999688,207.9375));
#22403=CARTESIAN_POINT('Origin',(313.2,2.72004641033163E-12,200.));
#22404=CARTESIAN_POINT('',(342.2,-2.38697950294409E-12,-154.2));
#22405=CARTESIAN_POINT('',(313.2,-2.22044604925031E-12,-172.2));
#22406=CARTESIAN_POINT('',(342.2,-2.38697950294409E-12,-172.2));
#22407=CARTESIAN_POINT('',(313.2,2.72004641033163E-12,200.));
#22408=CARTESIAN_POINT('',(250.,3.1641356201817E-12,200.));
#22409=CARTESIAN_POINT('',(342.2,-2.44249065417534E-12,172.2));
#22410=CARTESIAN_POINT('',(342.2,-2.33146835171283E-12,154.2));
#22411=CARTESIAN_POINT('Origin',(250.,3.1641356201817E-12,200.));
#22412=CARTESIAN_POINT('',(250.,-63.1999999999969,200.));
#22413=CARTESIAN_POINT('Origin',(250.,-63.1999999999969,200.));
#22414=CARTESIAN_POINT('',(250.2,-63.1999999999969,200.));
#22415=CARTESIAN_POINT('Origin',(250.2,-55.4624999999969,200.));
#22416=CARTESIAN_POINT('',(257.9375,-55.4624999999969,200.));
#22417=CARTESIAN_POINT('Origin',(257.9375,-55.4624999999969,200.));
#22418=CARTESIAN_POINT('',(257.9375,-15.8749999999969,200.));
#22419=CARTESIAN_POINT('Origin',(265.875,-15.874999999997,200.));
#22420=CARTESIAN_POINT('',(265.875,-7.93749999999693,200.));
#22421=CARTESIAN_POINT('Origin',(265.875,-7.93749999999699,200.));
#22422=CARTESIAN_POINT('',(265.875,-7.93749999999693,-154.2));
#22423=CARTESIAN_POINT('',(265.875,-7.93749999999688,154.2));
#22424=CARTESIAN_POINT('',(265.875,-7.93749999999699,172.2));
#22425=CARTESIAN_POINT('',(305.4625,-7.93749999999727,-172.2));
#22426=CARTESIAN_POINT('',(305.4625,-7.93749999999721,200.));
#22427=CARTESIAN_POINT('',(265.875,-7.93749999999693,-172.2));
#22428=CARTESIAN_POINT('Origin',(305.4625,-0.199999999997258,200.));
#22429=CARTESIAN_POINT('',(313.2,-0.199999999997258,-172.2));
#22430=CARTESIAN_POINT('Origin',(305.4625,-0.199999999997258,-172.2));
#22431=CARTESIAN_POINT('',(313.2,-0.199999999997258,200.));
#22432=CARTESIAN_POINT('Origin',(313.2,2.72004641033163E-12,200.));
#22433=CARTESIAN_POINT('',(313.2,2.72004641033163E-12,-172.2));
#22434=CARTESIAN_POINT('Origin',(342.2,-10.0000000000024,172.2));
#22435=CARTESIAN_POINT('Origin',(342.2,-10.0000000000023,154.2));
#22436=CARTESIAN_POINT('Origin',(342.2,-10.0000000000024,-154.2));
#22437=CARTESIAN_POINT('Origin',(342.2,-10.0000000000024,-172.2));
#22438=CARTESIAN_POINT('Origin',(286.9375,-36.9374999999999,147.85));
#22439=CARTESIAN_POINT('',(295.9375,-36.9374999999999,147.85));
#22440=CARTESIAN_POINT('Origin',(286.9375,-36.9374999999999,147.85));
#22441=CARTESIAN_POINT('',(295.9375,-36.9374999999999,154.2));
#22442=CARTESIAN_POINT('',(295.9375,-36.9374999999999,147.85));
#22443=CARTESIAN_POINT('Origin',(286.9375,-36.9374999999999,154.2));
#22444=CARTESIAN_POINT('Origin',(286.9375,-36.9374999999999,147.85));
#22445=CARTESIAN_POINT('',(265.875,-7.93749999999988,147.85));
#22446=CARTESIAN_POINT('',(257.9375,-15.8749999999969,147.85));
#22447=CARTESIAN_POINT('',(257.9375,-15.8749999999969,147.85));
#22448=CARTESIAN_POINT('',(305.9375,-7.93749999999988,147.85));
#22449=CARTESIAN_POINT('',(265.875,-7.93749999999988,147.85));
#22450=CARTESIAN_POINT('',(305.9375,-36.9374999999999,147.85));
#22451=CARTESIAN_POINT('',(305.9375,-7.93749999999988,147.85));
#22452=CARTESIAN_POINT('',(286.9375,-55.9374999999999,147.85));
#22453=CARTESIAN_POINT('Origin',(286.9375,-36.9374999999999,147.85));
#22454=CARTESIAN_POINT('',(257.9375,-55.9374999999999,147.85));
#22455=CARTESIAN_POINT('',(286.9375,-55.9374999999999,147.85));
#22456=CARTESIAN_POINT('',(257.9375,-55.9374999999999,147.85));
#22457=CARTESIAN_POINT('Origin',(286.9375,-36.9374999999999,154.2));
#22458=CARTESIAN_POINT('',(265.875,-7.93749999999988,154.2));
#22459=CARTESIAN_POINT('',(257.9375,-15.8749999999969,154.2));
#22460=CARTESIAN_POINT('',(257.9375,-15.8749999999969,154.2));
#22461=CARTESIAN_POINT('',(257.9375,-55.9374999999999,154.2));
#22462=CARTESIAN_POINT('',(257.9375,-55.9374999999999,154.2));
#22463=CARTESIAN_POINT('',(286.9375,-55.9374999999999,154.2));
#22464=CARTESIAN_POINT('',(286.9375,-55.9374999999999,154.2));
#22465=CARTESIAN_POINT('',(305.9375,-36.9374999999999,154.2));
#22466=CARTESIAN_POINT('Origin',(286.9375,-36.9374999999999,154.2));
#22467=CARTESIAN_POINT('',(305.9375,-7.93749999999988,154.2));
#22468=CARTESIAN_POINT('',(305.9375,-7.93749999999988,154.2));
#22469=CARTESIAN_POINT('',(265.875,-7.93749999999988,154.2));
#22470=CARTESIAN_POINT('Origin',(257.9375,-15.8749999999969,147.85));
#22471=CARTESIAN_POINT('',(265.875,-7.93749999999988,147.85));
#22472=CARTESIAN_POINT('',(257.9375,-15.8749999999969,147.85));
#22473=CARTESIAN_POINT('Origin',(257.9375,-55.9374999999999,147.85));
#22474=CARTESIAN_POINT('',(257.9375,-55.9374999999999,147.85));
#22475=CARTESIAN_POINT('Origin',(286.9375,-55.9374999999999,147.85));
#22476=CARTESIAN_POINT('',(286.9375,-55.9374999999999,147.85));
#22477=CARTESIAN_POINT('Origin',(286.9375,-36.9374999999999,147.85));
#22478=CARTESIAN_POINT('',(305.9375,-36.9374999999999,147.85));
#22479=CARTESIAN_POINT('Origin',(305.9375,-7.93749999999988,147.85));
#22480=CARTESIAN_POINT('',(305.9375,-7.93749999999988,147.85));
#22481=CARTESIAN_POINT('Origin',(265.875,-7.93749999999988,147.85));
#22482=CARTESIAN_POINT('Origin',(286.9375,-36.9375,-147.85));
#22483=CARTESIAN_POINT('',(295.9375,-36.9375,-147.85));
#22484=CARTESIAN_POINT('Origin',(286.9375,-36.9375,-147.85));
#22485=CARTESIAN_POINT('',(295.9375,-36.9375,-154.2));
#22486=CARTESIAN_POINT('',(295.9375,-36.9375,-147.85));
#22487=CARTESIAN_POINT('Origin',(286.9375,-36.9375,-154.2));
#22488=CARTESIAN_POINT('Origin',(286.9375,-36.9375,-147.85));
#22489=CARTESIAN_POINT('',(265.875,-7.93749999999999,-147.85));
#22490=CARTESIAN_POINT('',(257.9375,-15.8749999999969,-147.85));
#22491=CARTESIAN_POINT('',(257.9375,-15.8749999999969,-147.85));
#22492=CARTESIAN_POINT('',(257.9375,-55.9375,-147.85));
#22493=CARTESIAN_POINT('',(257.9375,-55.9375,-147.85));
#22494=CARTESIAN_POINT('',(286.9375,-55.9375,-147.85));
#22495=CARTESIAN_POINT('',(286.9375,-55.9375,-147.85));
#22496=CARTESIAN_POINT('',(305.9375,-36.9375,-147.85));
#22497=CARTESIAN_POINT('Origin',(286.9375,-36.9375,-147.85));
#22498=CARTESIAN_POINT('',(305.9375,-7.93749999999999,-147.85));
#22499=CARTESIAN_POINT('',(305.9375,-7.93749999999999,-147.85));
#22500=CARTESIAN_POINT('',(265.875,-7.93749999999999,-147.85));
#22501=CARTESIAN_POINT('Origin',(286.9375,-36.9375,-154.2));
#22502=CARTESIAN_POINT('',(265.875,-7.93749999999999,-154.2));
#22503=CARTESIAN_POINT('',(257.9375,-15.874999999997,-154.2));
#22504=CARTESIAN_POINT('',(257.9375,-15.874999999997,-154.2));
#22505=CARTESIAN_POINT('',(305.9375,-7.93749999999999,-154.2));
#22506=CARTESIAN_POINT('',(265.875,-7.93749999999999,-154.2));
#22507=CARTESIAN_POINT('',(305.9375,-36.9375,-154.2));
#22508=CARTESIAN_POINT('',(305.9375,-7.93749999999999,-154.2));
#22509=CARTESIAN_POINT('',(286.9375,-55.9375,-154.2));
#22510=CARTESIAN_POINT('Origin',(286.9375,-36.9375,-154.2));
#22511=CARTESIAN_POINT('',(257.9375,-55.9375,-154.2));
#22512=CARTESIAN_POINT('',(286.9375,-55.9375,-154.2));
#22513=CARTESIAN_POINT('',(257.9375,-55.9375,-154.2));
#22514=CARTESIAN_POINT('Origin',(257.9375,-15.8749999999969,-147.85));
#22515=CARTESIAN_POINT('',(257.9375,-15.8749999999969,-147.85));
#22516=CARTESIAN_POINT('',(265.875,-7.93749999999999,-147.85));
#22517=CARTESIAN_POINT('Origin',(257.9375,-55.9375,-147.85));
#22518=CARTESIAN_POINT('',(257.9375,-55.9375,-147.85));
#22519=CARTESIAN_POINT('Origin',(286.9375,-55.9375,-147.85));
#22520=CARTESIAN_POINT('',(286.9375,-55.9375,-147.85));
#22521=CARTESIAN_POINT('Origin',(286.9375,-36.9375,-147.85));
#22522=CARTESIAN_POINT('',(305.9375,-36.9375,-147.85));
#22523=CARTESIAN_POINT('Origin',(305.9375,-7.93749999999999,-147.85));
#22524=CARTESIAN_POINT('',(305.9375,-7.93749999999999,-147.85));
#22525=CARTESIAN_POINT('Origin',(265.875,-7.93749999999999,-147.85));
#22526=CARTESIAN_POINT('',(0.,0.,0.));
#22527=CARTESIAN_POINT('Origin',(314.,-7.9375,-264.));
#22528=CARTESIAN_POINT('',(314.,0.,-172.));
#22529=CARTESIAN_POINT('',(314.,0.,-264.));
#22530=CARTESIAN_POINT('',(314.,0.,-264.));
#22531=CARTESIAN_POINT('',(314.,-7.9375,-172.));
#22532=CARTESIAN_POINT('',(314.,-7.9375,-172.));
#22533=CARTESIAN_POINT('',(314.,-7.9375,-264.));
#22534=CARTESIAN_POINT('',(314.,-7.9375,-264.));
#22535=CARTESIAN_POINT('',(314.,-7.9375,-264.));
#22536=CARTESIAN_POINT('Origin',(314.,-7.9375,-172.));
#22537=CARTESIAN_POINT('',(285.,0.,-172.));
#22538=CARTESIAN_POINT('',(314.,0.,-172.));
#22539=CARTESIAN_POINT('',(285.,-7.9375,-172.));
#22540=CARTESIAN_POINT('',(285.,-7.9375,-172.));
#22541=CARTESIAN_POINT('',(314.,-7.9375,-172.));
#22542=CARTESIAN_POINT('Origin',(285.,-7.9375,-163.));
#22543=CARTESIAN_POINT('',(285.,0.,-154.));
#22544=CARTESIAN_POINT('Origin',(285.,0.,-163.));
#22545=CARTESIAN_POINT('',(285.,-7.9375,-154.));
#22546=CARTESIAN_POINT('',(285.,-7.9375,-154.));
#22547=CARTESIAN_POINT('Origin',(285.,-7.9375,-163.));
#22548=CARTESIAN_POINT('Origin',(285.,-7.9375,-154.));
#22549=CARTESIAN_POINT('',(314.,0.,-154.));
#22550=CARTESIAN_POINT('',(285.,0.,-154.));
#22551=CARTESIAN_POINT('',(314.,-7.9375,-154.));
#22552=CARTESIAN_POINT('',(314.,-7.9375,-154.));
#22553=CARTESIAN_POINT('',(285.,-7.9375,-154.));
#22554=CARTESIAN_POINT('Origin',(314.,-7.9375,-154.));
#22555=CARTESIAN_POINT('',(314.,0.,154.));
#22556=CARTESIAN_POINT('',(314.,0.,-154.));
#22557=CARTESIAN_POINT('',(314.,-7.9375,154.));
#22558=CARTESIAN_POINT('',(314.,-7.9375,154.));
#22559=CARTESIAN_POINT('',(314.,-7.9375,-154.));
#22560=CARTESIAN_POINT('Origin',(314.,-7.9375,154.));
#22561=CARTESIAN_POINT('',(285.,0.,154.));
#22562=CARTESIAN_POINT('',(314.,0.,154.));
#22563=CARTESIAN_POINT('',(285.,-7.9375,154.));
#22564=CARTESIAN_POINT('',(285.,-7.9375,154.));
#22565=CARTESIAN_POINT('',(314.,-7.9375,154.));
#22566=CARTESIAN_POINT('Origin',(285.,-7.9375,163.));
#22567=CARTESIAN_POINT('',(285.,0.,172.));
#22568=CARTESIAN_POINT('Origin',(285.,0.,163.));
#22569=CARTESIAN_POINT('',(285.,-7.9375,172.));
#22570=CARTESIAN_POINT('',(285.,-7.9375,172.));
#22571=CARTESIAN_POINT('Origin',(285.,-7.9375,163.));
#22572=CARTESIAN_POINT('Origin',(285.,-7.9375,172.));
#22573=CARTESIAN_POINT('',(314.,0.,172.));
#22574=CARTESIAN_POINT('',(285.,0.,172.));
#22575=CARTESIAN_POINT('',(314.,-7.9375,172.));
#22576=CARTESIAN_POINT('',(314.,-7.9375,172.));
#22577=CARTESIAN_POINT('',(285.,-7.9375,172.));
#22578=CARTESIAN_POINT('Origin',(314.,-7.9375,172.));
#22579=CARTESIAN_POINT('',(314.,0.,264.));
#22580=CARTESIAN_POINT('',(314.,0.,172.));
#22581=CARTESIAN_POINT('',(314.,-7.9375,264.));
#22582=CARTESIAN_POINT('',(314.,-7.9375,264.));
#22583=CARTESIAN_POINT('',(314.,-7.9375,172.));
#22584=CARTESIAN_POINT('Origin',(-314.,-7.9375,264.));
#22585=CARTESIAN_POINT('',(-314.,0.,264.));
#22586=CARTESIAN_POINT('',(-314.,0.,264.));
#22587=CARTESIAN_POINT('',(-314.,-7.9375,264.));
#22588=CARTESIAN_POINT('',(-314.,-7.9375,264.));
#22589=CARTESIAN_POINT('',(-314.,-7.9375,264.));
#22590=CARTESIAN_POINT('Origin',(-314.,-7.9375,264.));
#22591=CARTESIAN_POINT('',(-314.,0.,-264.));
#22592=CARTESIAN_POINT('',(-314.,0.,264.));
#22593=CARTESIAN_POINT('',(-314.,-7.9375,-264.));
#22594=CARTESIAN_POINT('',(-314.,-7.9375,-264.));
#22595=CARTESIAN_POINT('',(-314.,-7.9375,264.));
#22596=CARTESIAN_POINT('Origin',(-314.,-7.9375,-264.));
#22597=CARTESIAN_POINT('',(-314.,0.,-264.));
#22598=CARTESIAN_POINT('',(-314.,-7.9375,-264.));
#22599=CARTESIAN_POINT('Origin',(285.,-7.9375,-163.));
#22600=CARTESIAN_POINT('Origin',(285.,0.,-163.));
#22601=CARTESIAN_POINT('Origin',(-340.832815729998,-8.,171.9375));
#22602=CARTESIAN_POINT('',(-331.832815729998,-8.,171.9375));
#22603=CARTESIAN_POINT('Origin',(-340.832815729998,-8.,171.9375));
#22604=CARTESIAN_POINT('',(-331.832815729998,-8.,164.));
#22605=CARTESIAN_POINT('',(-331.832815729998,-8.,171.9375));
#22606=CARTESIAN_POINT('Origin',(-340.832815729998,-8.,164.));
#22607=CARTESIAN_POINT('Origin',(-314.,-5.,171.9375));
#22608=CARTESIAN_POINT('',(-318.96903995,-5.55555555555555,171.9375));
#22609=CARTESIAN_POINT('',(-314.,0.,171.9375));
#22610=CARTESIAN_POINT('Origin',(-314.,-5.,171.9375));
#22611=CARTESIAN_POINT('',(-318.96903995,-5.55555555555555,164.));
#22612=CARTESIAN_POINT('',(-318.96903995,-5.55555555555555,171.9375));
#22613=CARTESIAN_POINT('',(-314.,0.,164.));
#22614=CARTESIAN_POINT('Origin',(-314.,-5.,164.));
#22615=CARTESIAN_POINT('',(-314.,0.,171.9375));
#22616=CARTESIAN_POINT('Origin',(-340.832815729998,-8.,171.9375));
#22617=CARTESIAN_POINT('',(-340.832815729998,14.,171.9375));
#22618=CARTESIAN_POINT('Origin',(-340.832815729998,-8.,171.9375));
#22619=CARTESIAN_POINT('',(-340.832815729998,14.,164.));
#22620=CARTESIAN_POINT('',(-340.832815729998,14.,171.9375));
#22621=CARTESIAN_POINT('Origin',(-340.832815729998,-8.,164.));
#22622=CARTESIAN_POINT('Origin',(-340.832815729998,-8.,171.9375));
#22623=CARTESIAN_POINT('',(-265.832815729998,0.,171.9375));
#22624=CARTESIAN_POINT('',(-265.832815729998,0.,171.9375));
#22625=CARTESIAN_POINT('',(-260.832815729998,5.,171.9375));
#22626=CARTESIAN_POINT('',(-260.832815729998,5.,171.9375));
#22627=CARTESIAN_POINT('',(-260.832815729998,14.,171.9375));
#22628=CARTESIAN_POINT('',(-260.832815729998,14.,171.9375));
#22629=CARTESIAN_POINT('',(-340.832815729998,14.,171.9375));
#22630=CARTESIAN_POINT('Origin',(-340.832815729998,-8.,164.));
#22631=CARTESIAN_POINT('',(-260.832815729998,14.,164.));
#22632=CARTESIAN_POINT('',(-340.832815729998,14.,164.));
#22633=CARTESIAN_POINT('',(-260.832815729998,5.,164.));
#22634=CARTESIAN_POINT('',(-260.832815729998,14.,164.));
#22635=CARTESIAN_POINT('',(-265.832815729998,0.,164.));
#22636=CARTESIAN_POINT('',(-260.832815729998,5.,164.));
#22637=CARTESIAN_POINT('',(-265.832815729998,0.,164.));
#22638=CARTESIAN_POINT('Origin',(-265.832815729998,0.,171.9375));
#22639=CARTESIAN_POINT('',(-265.832815729998,0.,171.9375));
#22640=CARTESIAN_POINT('Origin',(-260.832815729998,5.,171.9375));
#22641=CARTESIAN_POINT('',(-260.832815729998,5.,171.9375));
#22642=CARTESIAN_POINT('Origin',(-260.832815729998,14.,171.9375));
#22643=CARTESIAN_POINT('',(-260.832815729998,14.,171.9375));
#22644=CARTESIAN_POINT('Origin',(-340.832815729998,14.,171.9375));
#22645=CARTESIAN_POINT('Origin',(-340.832815729998,-8.,-171.9375));
#22646=CARTESIAN_POINT('',(-331.832815729998,-8.,-171.9375));
#22647=CARTESIAN_POINT('Origin',(-340.832815729998,-8.,-171.9375));
#22648=CARTESIAN_POINT('',(-331.832815729998,-8.,-164.));
#22649=CARTESIAN_POINT('',(-331.832815729998,-8.,-171.9375));
#22650=CARTESIAN_POINT('Origin',(-340.832815729998,-8.,-164.));
#22651=CARTESIAN_POINT('Origin',(-314.,-5.,-171.9375));
#22652=CARTESIAN_POINT('',(-318.96903995,-5.55555555555555,-171.9375));
#22653=CARTESIAN_POINT('',(-314.,0.,-171.9375));
#22654=CARTESIAN_POINT('Origin',(-314.,-5.,-171.9375));
#22655=CARTESIAN_POINT('',(-314.,0.,-164.));
#22656=CARTESIAN_POINT('',(-314.,0.,-171.9375));
#22657=CARTESIAN_POINT('',(-318.96903995,-5.55555555555555,-164.));
#22658=CARTESIAN_POINT('Origin',(-314.,-5.,-164.));
#22659=CARTESIAN_POINT('',(-318.96903995,-5.55555555555555,-171.9375));
#22660=CARTESIAN_POINT('Origin',(-340.832815729998,-8.,-171.9375));
#22661=CARTESIAN_POINT('',(-340.832815729998,14.,-171.9375));
#22662=CARTESIAN_POINT('Origin',(-340.832815729998,-8.,-171.9375));
#22663=CARTESIAN_POINT('',(-340.832815729998,14.,-164.));
#22664=CARTESIAN_POINT('Origin',(-340.832815729998,-8.,-164.));
#22665=CARTESIAN_POINT('',(-340.832815729998,14.,-171.9375));
#22666=CARTESIAN_POINT('Origin',(-340.832815729998,-8.,-171.9375));
#22667=CARTESIAN_POINT('',(-260.832815729998,14.,-171.9375));
#22668=CARTESIAN_POINT('',(-340.832815729998,14.,-171.9375));
#22669=CARTESIAN_POINT('',(-260.832815729998,5.,-171.9375));
#22670=CARTESIAN_POINT('',(-260.832815729998,14.,-171.9375));
#22671=CARTESIAN_POINT('',(-265.832815729998,0.,-171.9375));
#22672=CARTESIAN_POINT('',(-260.832815729998,5.,-171.9375));
#22673=CARTESIAN_POINT('',(-265.832815729998,0.,-171.9375));
#22674=CARTESIAN_POINT('Origin',(-340.832815729998,-8.,-164.));
#22675=CARTESIAN_POINT('',(-265.832815729998,0.,-164.));
#22676=CARTESIAN_POINT('',(-265.832815729998,0.,-164.));
#22677=CARTESIAN_POINT('',(-260.832815729998,5.,-164.));
#22678=CARTESIAN_POINT('',(-260.832815729998,5.,-164.));
#22679=CARTESIAN_POINT('',(-260.832815729998,14.,-164.));
#22680=CARTESIAN_POINT('',(-260.832815729998,14.,-164.));
#22681=CARTESIAN_POINT('',(-340.832815729998,14.,-164.));
#22682=CARTESIAN_POINT('Origin',(-265.832815729998,0.,-171.9375));
#22683=CARTESIAN_POINT('',(-265.832815729998,0.,-171.9375));
#22684=CARTESIAN_POINT('Origin',(-260.832815729998,5.,-171.9375));
#22685=CARTESIAN_POINT('',(-260.832815729998,5.,-171.9375));
#22686=CARTESIAN_POINT('Origin',(-260.832815729998,14.,-171.9375));
#22687=CARTESIAN_POINT('',(-260.832815729998,14.,-171.9375));
#22688=CARTESIAN_POINT('Origin',(-340.832815729998,14.,-171.9375));
#22689=CARTESIAN_POINT('Origin',(250.,49.,44.));
#22690=CARTESIAN_POINT('',(257.9375,60.,44.));
#22691=CARTESIAN_POINT('',(250.,52.0625,44.));
#22692=CARTESIAN_POINT('Origin',(250.,60.,44.));
#22693=CARTESIAN_POINT('',(250.,49.,47.0625));
#22694=CARTESIAN_POINT('Origin',(250.,49.,44.));
#22695=CARTESIAN_POINT('Origin',(250.,49.,55.));
#22696=CARTESIAN_POINT('Origin',(250.,60.,44.));
#22697=CARTESIAN_POINT('Origin',(250.,49.,-44.));
#22698=CARTESIAN_POINT('',(250.,49.,-47.0625));
#22699=CARTESIAN_POINT('Origin',(250.,49.,-55.));
#22700=CARTESIAN_POINT('',(250.,52.0625,-44.));
#22701=CARTESIAN_POINT('Origin',(250.,49.,-44.));
#22702=CARTESIAN_POINT('',(257.9375,60.,-44.));
#22703=CARTESIAN_POINT('Origin',(250.,60.,-44.));
#22704=CARTESIAN_POINT('Origin',(250.,60.,-44.));
#22705=CARTESIAN_POINT('Origin',(250.,0.,55.));
#22706=CARTESIAN_POINT('',(250.,9.71612661605436E-16,47.0625));
#22707=CARTESIAN_POINT('',(250.,1.12403000739313E-15,47.0625));
#22708=CARTESIAN_POINT('Origin',(250.,0.,55.));
#22709=CARTESIAN_POINT('Origin',(250.,60.,44.));
#22710=CARTESIAN_POINT('',(257.9375,60.,44.));
#22711=CARTESIAN_POINT('Origin',(250.,49.,-55.));
#22712=CARTESIAN_POINT('',(250.,0.,-47.0625));
#22713=CARTESIAN_POINT('Origin',(250.,0.,-55.));
#22714=CARTESIAN_POINT('',(250.,49.,-47.0625));
#22715=CARTESIAN_POINT('Origin',(250.,0.,-55.));
#22716=CARTESIAN_POINT('Origin',(250.,0.,55.));
#22717=CARTESIAN_POINT('',(0.,0.,0.));
#22718=CARTESIAN_POINT('Origin',(55.7276,0.,0.));
#22719=CARTESIAN_POINT('',(54.88813,-9.72063396823211E-16,-7.9375));
#22720=CARTESIAN_POINT('Origin',(54.88813,0.,0.));
#22721=CARTESIAN_POINT('',(55.7276,-8.69257971975189E-16,-7.09803));
#22722=CARTESIAN_POINT('',(55.7276,-8.69257971975189E-16,-7.09803));
#22723=CARTESIAN_POINT('Origin',(55.7276,0.,0.));
#22724=CARTESIAN_POINT('Origin',(0.,0.,0.));
#22725=CARTESIAN_POINT('',(11.2776,-9.72063396823212E-16,-7.9375));
#22726=CARTESIAN_POINT('Origin',(11.2776,0.,0.));
#22727=CARTESIAN_POINT('',(0.,-9.72063396823212E-16,-7.9375));
#22728=CARTESIAN_POINT('Origin',(11.2776,7.78695402066815,-13.4874));
#22729=CARTESIAN_POINT('',(1.20464597933184,15.5739080413363,-7.15323062778294E-16));
#22730=CARTESIAN_POINT('',(0.,11.6804310310022,-6.74370000000001));
#22731=CARTESIAN_POINT('Ctrl Pts',(1.20464597933472,15.5739080413413,8.62256231748444E-12));
#22732=CARTESIAN_POINT('Ctrl Pts',(5.88418203051333E-15,13.487400000002,
-3.61393793799207));
#22733=CARTESIAN_POINT('Ctrl Pts',(5.21480900164849E-15,11.6804310310022,
-6.74370000000001));
#22734=CARTESIAN_POINT('',(11.2776,15.5739080413363,0.));
#22735=CARTESIAN_POINT('',(11.2776,15.5739080413363,0.));
#22736=CARTESIAN_POINT('',(11.2776,7.78695402066815,-13.4874));
#22737=CARTESIAN_POINT('',(11.2776,7.78695402066815,-13.4874));
#22738=CARTESIAN_POINT('',(1.20464597933183,7.78695402066815,-13.4874));
#22739=CARTESIAN_POINT('',(11.2776,7.78695402066815,-13.4874));
#22740=CARTESIAN_POINT('Ctrl Pts',(5.21480900164849E-15,11.6804310310022,
-6.74370000000001));
#22741=CARTESIAN_POINT('Ctrl Pts',(4.72325692176463E-15,9.87346206200247,
-9.87346206200795));
#22742=CARTESIAN_POINT('Ctrl Pts',(1.20464597933471,7.78695402066317,-13.4874000000086));
#22743=CARTESIAN_POINT('Origin',(11.2776,15.5739080413363,0.));
#22744=CARTESIAN_POINT('',(1.20464597933183,7.78695402066815,13.4874));
#22745=CARTESIAN_POINT('',(0.,11.6804310310022,6.74370000000002));
#22746=CARTESIAN_POINT('Ctrl Pts',(1.2046459793347,7.78695402066317,13.4874000000086));
#22747=CARTESIAN_POINT('Ctrl Pts',(4.44089209850063E-16,9.87346206200247,
9.87346206200795));
#22748=CARTESIAN_POINT('Ctrl Pts',(2.75695286792984E-32,11.6804310310022,
6.74370000000002));
#22749=CARTESIAN_POINT('',(11.2776,7.78695402066815,13.4874));
#22750=CARTESIAN_POINT('',(11.2776,7.78695402066815,13.4874));
#22751=CARTESIAN_POINT('',(11.2776,15.5739080413363,0.));
#22752=CARTESIAN_POINT('Ctrl Pts',(2.75695286792984E-32,11.6804310310022,
6.74370000000002));
#22753=CARTESIAN_POINT('Ctrl Pts',(1.64432633682228E-32,13.487400000002,
3.61393793799206));
#22754=CARTESIAN_POINT('Ctrl Pts',(1.20464597933472,15.5739080413413,-8.63647399109626E-12));
#22755=CARTESIAN_POINT('Origin',(11.2776,7.78695402066815,13.4874));
#22756=CARTESIAN_POINT('',(1.20464597933184,-7.78695402066817,13.4874));
#22757=CARTESIAN_POINT('',(0.,1.50231459873716E-15,13.4874));
#22758=CARTESIAN_POINT('Ctrl Pts',(1.20464597933471,-7.78695402067813,13.4874));
#22759=CARTESIAN_POINT('Ctrl Pts',(-2.88657986402541E-15,-3.61393793799953,
13.4874));
#22760=CARTESIAN_POINT('Ctrl Pts',(-3.47653933443233E-15,-1.9865939053899E-15,
13.4874));
#22761=CARTESIAN_POINT('',(11.2776,-7.78695402066817,13.4874));
#22762=CARTESIAN_POINT('',(11.2776,-7.78695402066817,13.4874));
#22763=CARTESIAN_POINT('',(11.2776,7.78695402066815,13.4874));
#22764=CARTESIAN_POINT('Ctrl Pts',(-3.47653933443233E-15,-1.9865939053899E-15,
13.4874));
#22765=CARTESIAN_POINT('Ctrl Pts',(-3.86572425055132E-15,3.61393793799952,
13.4874));
#22766=CARTESIAN_POINT('Ctrl Pts',(1.2046459793347,7.7869540206781,13.4874));
#22767=CARTESIAN_POINT('Origin',(11.2776,-15.5739080413363,2.70693809272771E-16));
#22768=CARTESIAN_POINT('',(1.20464597933185,-15.5739080413363,4.81312603749133E-16));
#22769=CARTESIAN_POINT('',(0.,-11.6804310310022,6.74370000000001));
#22770=CARTESIAN_POINT('Ctrl Pts',(1.20464597933473,-15.5739080413413,-8.62951815429035E-12));
#22771=CARTESIAN_POINT('Ctrl Pts',(1.0325074129014E-14,-13.487400000002,
3.61393793799206));
#22772=CARTESIAN_POINT('Ctrl Pts',(8.44302409790707E-15,-11.6804310310023,
6.74370000000001));
#22773=CARTESIAN_POINT('',(11.2776,-15.5739080413363,2.70693809272771E-16));
#22774=CARTESIAN_POINT('',(11.2776,-15.5739080413363,2.70693809272771E-16));
#22775=CARTESIAN_POINT('',(11.2776,-15.5739080413363,2.70693809272771E-16));
#22776=CARTESIAN_POINT('Ctrl Pts',(8.44302409790707E-15,-11.6804310310023,
6.74370000000001));
#22777=CARTESIAN_POINT('Ctrl Pts',(6.29021451463548E-15,-9.87346206200249,
9.87346206200794));
#22778=CARTESIAN_POINT('Ctrl Pts',(1.20464597933471,-7.7869540206632,13.4874000000086));
#22779=CARTESIAN_POINT('Origin',(11.2776,-7.78695402066818,-13.4874));
#22780=CARTESIAN_POINT('',(1.20464597933184,-7.78695402066818,-13.4874));
#22781=CARTESIAN_POINT('',(0.,-11.6804310310022,-6.74370000000001));
#22782=CARTESIAN_POINT('Ctrl Pts',(1.20464597933471,-7.78695402066319,-13.4874000000086));
#22783=CARTESIAN_POINT('Ctrl Pts',(1.48769885299771E-14,-9.87346206200248,
-9.87346206200796));
#22784=CARTESIAN_POINT('Ctrl Pts',(1.24162119086869E-14,-11.6804310310022,
-6.74370000000003));
#22785=CARTESIAN_POINT('',(11.2776,-7.78695402066818,-13.4874));
#22786=CARTESIAN_POINT('',(11.2776,-7.78695402066818,-13.4874));
#22787=CARTESIAN_POINT('',(11.2776,-7.78695402066818,-13.4874));
#22788=CARTESIAN_POINT('Ctrl Pts',(1.24162119086869E-14,-11.6804310310022,
-6.74370000000003));
#22789=CARTESIAN_POINT('Ctrl Pts',(1.02729326886213E-14,-13.487400000002,
-3.61393793799208));
#22790=CARTESIAN_POINT('Ctrl Pts',(1.20464597933472,-15.5739080413413,8.60758051513325E-12));
#22791=CARTESIAN_POINT('Origin',(11.2776,7.78695402066815,-13.4874));
#22792=CARTESIAN_POINT('',(0.,3.00462919747432E-15,-13.4874));
#22793=CARTESIAN_POINT('Ctrl Pts',(1.20464597933471,7.78695402067811,-13.4874));
#22794=CARTESIAN_POINT('Ctrl Pts',(2.66453525910038E-15,3.61393793799952,
-13.4874));
#22795=CARTESIAN_POINT('Ctrl Pts',(2.48324238173738E-15,0.,-13.4874));
#22796=CARTESIAN_POINT('',(11.2776,7.78695402066815,-13.4874));
#22797=CARTESIAN_POINT('Ctrl Pts',(2.48324238173738E-15,0.,-13.4874));
#22798=CARTESIAN_POINT('Ctrl Pts',(2.55640694962002E-15,-3.61393793799953,
-13.4874));
#22799=CARTESIAN_POINT('Ctrl Pts',(1.20464597933471,-7.78695402067813,-13.4874));
#22800=CARTESIAN_POINT('Origin',(11.2776,15.5739080413363,1.3010426069826E-15));
#22801=CARTESIAN_POINT('Origin',(55.7276,0.,0.));
#22802=CARTESIAN_POINT('Origin',(0.,0.,0.));
#22803=CARTESIAN_POINT('Origin',(0.,0.,0.));
#22804=CARTESIAN_POINT('Origin',(0.,0.,0.));
#22805=CARTESIAN_POINT('Origin',(0.,0.,0.));
#22806=CARTESIAN_POINT('Origin',(0.,0.,0.));
#22807=CARTESIAN_POINT('Origin',(0.,0.,0.));
#22808=CARTESIAN_POINT('Origin',(0.,0.,0.));
#22809=CARTESIAN_POINT('Origin',(0.,0.,0.));
#22810=CARTESIAN_POINT('Origin',(0.,0.,0.));
#22811=CARTESIAN_POINT('Origin',(0.,0.,0.));
#22812=CARTESIAN_POINT('Origin',(0.,0.,0.));
#22813=CARTESIAN_POINT('Origin',(0.,0.,0.));
#22814=CARTESIAN_POINT('Origin',(0.,15.5739080413363,1.3010426069826E-15));
#22815=CARTESIAN_POINT('',(0.,0.,0.));
#22816=CARTESIAN_POINT('Origin',(74.7776,0.,0.));
#22817=CARTESIAN_POINT('',(73.93813,-9.72063396823212E-16,-7.93750000000001));
#22818=CARTESIAN_POINT('Origin',(73.93813,0.,0.));
#22819=CARTESIAN_POINT('',(74.7776,-8.69257971975189E-16,-7.09803));
#22820=CARTESIAN_POINT('',(74.7776,-8.69257971975189E-16,-7.09803));
#22821=CARTESIAN_POINT('Origin',(74.7776,0.,0.));
#22822=CARTESIAN_POINT('Origin',(0.,0.,0.));
#22823=CARTESIAN_POINT('',(11.2776,-9.72063396823212E-16,-7.9375));
#22824=CARTESIAN_POINT('Origin',(11.2776,0.,0.));
#22825=CARTESIAN_POINT('',(0.,-9.72063396823212E-16,-7.9375));
#22826=CARTESIAN_POINT('Origin',(11.2776,7.78695402066815,-13.4874));
#22827=CARTESIAN_POINT('',(1.20464597933184,15.5739080413363,-3.66756626076851E-16));
#22828=CARTESIAN_POINT('',(0.,11.6804310310022,-6.74370000000002));
#22829=CARTESIAN_POINT('Ctrl Pts',(1.20464597933471,15.5739080413413,8.62737789681159E-12));
#22830=CARTESIAN_POINT('Ctrl Pts',(-9.65894031423886E-15,13.487400000002,
-3.61393793799208));
#22831=CARTESIAN_POINT('Ctrl Pts',(-5.4631332398222E-15,11.6804310310022,
-6.74370000000003));
#22832=CARTESIAN_POINT('',(11.2776,15.5739080413363,0.));
#22833=CARTESIAN_POINT('',(11.2776,15.5739080413363,0.));
#22834=CARTESIAN_POINT('',(11.2776,7.78695402066815,-13.4874));
#22835=CARTESIAN_POINT('',(11.2776,7.78695402066815,-13.4874));
#22836=CARTESIAN_POINT('',(1.20464597933183,7.78695402066815,-13.4874));
#22837=CARTESIAN_POINT('',(11.2776,7.78695402066815,-13.4874));
#22838=CARTESIAN_POINT('Ctrl Pts',(-5.4631332398222E-15,11.6804310310022,
-6.74370000000003));
#22839=CARTESIAN_POINT('Ctrl Pts',(-1.64537630913334E-15,9.87346206200246,
-9.87346206200795));
#22840=CARTESIAN_POINT('Ctrl Pts',(1.2046459793347,7.78695402066317,-13.4874000000086));
#22841=CARTESIAN_POINT('Origin',(11.2776,15.5739080413363,0.));
#22842=CARTESIAN_POINT('',(1.20464597933183,7.78695402066815,13.4874));
#22843=CARTESIAN_POINT('',(0.,11.6804310310022,6.74370000000002));
#22844=CARTESIAN_POINT('Ctrl Pts',(1.2046459793347,7.78695402066316,13.4874000000086));
#22845=CARTESIAN_POINT('Ctrl Pts',(3.33066907387547E-16,9.87346206200246,
9.87346206200796));
#22846=CARTESIAN_POINT('Ctrl Pts',(4.96648476347475E-16,11.6804310310022,
6.74370000000002));
#22847=CARTESIAN_POINT('',(11.2776,7.78695402066815,13.4874));
#22848=CARTESIAN_POINT('',(11.2776,7.78695402066815,13.4874));
#22849=CARTESIAN_POINT('',(11.2776,15.5739080413363,0.));
#22850=CARTESIAN_POINT('Ctrl Pts',(4.96648476347475E-16,11.6804310310022,
6.74370000000002));
#22851=CARTESIAN_POINT('Ctrl Pts',(4.75437074788592E-16,13.487400000002,
3.61393793799208));
#22852=CARTESIAN_POINT('Ctrl Pts',(1.20464597933472,15.5739080413413,-8.6123960944604E-12));
#22853=CARTESIAN_POINT('Origin',(11.2776,7.78695402066815,13.4874));
#22854=CARTESIAN_POINT('',(1.20464597933183,-7.78695402066814,13.4874));
#22855=CARTESIAN_POINT('',(0.,3.00462919747433E-15,13.4874));
#22856=CARTESIAN_POINT('Ctrl Pts',(1.2046459793347,-7.78695402067809,13.4874));
#22857=CARTESIAN_POINT('Ctrl Pts',(-4.21884749357559E-15,-3.61393793799951,
13.4874));
#22858=CARTESIAN_POINT('Ctrl Pts',(-2.48324238173737E-15,1.39061573377293E-14,
13.4874));
#22859=CARTESIAN_POINT('',(11.2776,-7.78695402066814,13.4874));
#22860=CARTESIAN_POINT('',(11.2776,-7.78695402066814,13.4874));
#22861=CARTESIAN_POINT('',(11.2776,7.78695402066815,13.4874));
#22862=CARTESIAN_POINT('Ctrl Pts',(-2.48324238173737E-15,1.39061573377293E-14,
13.4874));
#22863=CARTESIAN_POINT('Ctrl Pts',(-1.12263434420355E-15,3.61393793799953,
13.4874));
#22864=CARTESIAN_POINT('Ctrl Pts',(1.2046459793347,7.7869540206781,13.4874));
#22865=CARTESIAN_POINT('Origin',(11.2776,-15.5739080413363,0.));
#22866=CARTESIAN_POINT('',(1.20464597933184,-15.5739080413363,3.75592506952845E-16));
#22867=CARTESIAN_POINT('',(0.,-11.6804310310022,6.74370000000003));
#22868=CARTESIAN_POINT('Ctrl Pts',(1.20464597933472,-15.5739080413413,-8.61774673815726E-12));
#22869=CARTESIAN_POINT('Ctrl Pts',(2.1094237467878E-15,-13.487400000002,
3.61393793799208));
#22870=CARTESIAN_POINT('Ctrl Pts',(4.96648476347477E-16,-11.6804310310022,
6.74370000000002));
#22871=CARTESIAN_POINT('',(11.2776,-15.5739080413363,0.));
#22872=CARTESIAN_POINT('',(11.2776,-15.5739080413363,0.));
#22873=CARTESIAN_POINT('',(11.2776,-15.5739080413363,0.));
#22874=CARTESIAN_POINT('Ctrl Pts',(4.96648476347477E-16,-11.6804310310022,
6.74370000000002));
#22875=CARTESIAN_POINT('Ctrl Pts',(-9.58335530627874E-16,-9.87346206200246,
9.87346206200795));
#22876=CARTESIAN_POINT('Ctrl Pts',(1.2046459793347,-7.78695402066317,13.4874000000086));
#22877=CARTESIAN_POINT('Origin',(11.2776,-7.78695402066817,-13.4874));
#22878=CARTESIAN_POINT('',(1.20464597933184,-7.78695402066817,-13.4874));
#22879=CARTESIAN_POINT('',(0.,-11.6804310310022,-6.7437));
#22880=CARTESIAN_POINT('Ctrl Pts',(1.20464597933471,-7.7869540206632,-13.4874000000086));
#22881=CARTESIAN_POINT('Ctrl Pts',(8.43769498715119E-15,-9.87346206200249,
-9.87346206200795));
#22882=CARTESIAN_POINT('Ctrl Pts',(8.93967257425456E-15,-11.6804310310023,
-6.74370000000001));
#22883=CARTESIAN_POINT('',(11.2776,-7.78695402066817,-13.4874));
#22884=CARTESIAN_POINT('',(11.2776,-7.78695402066817,-13.4874));
#22885=CARTESIAN_POINT('',(11.2776,-7.78695402066817,-13.4874));
#22886=CARTESIAN_POINT('Ctrl Pts',(8.93967257425456E-15,-11.6804310310023,
-6.74370000000001));
#22887=CARTESIAN_POINT('Ctrl Pts',(9.09553207322584E-15,-13.487400000002,
-3.61393793799206));
#22888=CARTESIAN_POINT('Ctrl Pts',(1.20464597933472,-15.5739080413413,8.63486879798721E-12));
#22889=CARTESIAN_POINT('Origin',(11.2776,7.78695402066815,-13.4874));
#22890=CARTESIAN_POINT('',(0.,1.50231459873716E-15,-13.4874));
#22891=CARTESIAN_POINT('Ctrl Pts',(1.2046459793347,7.7869540206781,-13.4874));
#22892=CARTESIAN_POINT('Ctrl Pts',(-2.55351295663786E-15,3.61393793799952,
-13.4874));
#22893=CARTESIAN_POINT('Ctrl Pts',(-2.23491814356364E-15,1.9865939053899E-15,
-13.4874));
#22894=CARTESIAN_POINT('',(11.2776,7.78695402066815,-13.4874));
#22895=CARTESIAN_POINT('Ctrl Pts',(-2.23491814356364E-15,1.9865939053899E-15,
-13.4874));
#22896=CARTESIAN_POINT('Ctrl Pts',(-2.22907762438719E-15,-3.61393793799953,
-13.4874));
#22897=CARTESIAN_POINT('Ctrl Pts',(1.20464597933471,-7.78695402067813,-13.4874));
#22898=CARTESIAN_POINT('Origin',(11.2776,15.5739080413363,-1.3010426069826E-15));
#22899=CARTESIAN_POINT('Origin',(74.7776,0.,0.));
#22900=CARTESIAN_POINT('Origin',(0.,0.,0.));
#22901=CARTESIAN_POINT('Origin',(0.,0.,0.));
#22902=CARTESIAN_POINT('Origin',(0.,0.,0.));
#22903=CARTESIAN_POINT('Origin',(0.,0.,0.));
#22904=CARTESIAN_POINT('Origin',(0.,0.,0.));
#22905=CARTESIAN_POINT('Origin',(0.,0.,0.));
#22906=CARTESIAN_POINT('Origin',(0.,0.,0.));
#22907=CARTESIAN_POINT('Origin',(0.,0.,0.));
#22908=CARTESIAN_POINT('Origin',(0.,0.,0.));
#22909=CARTESIAN_POINT('Origin',(0.,0.,0.));
#22910=CARTESIAN_POINT('Origin',(0.,0.,0.));
#22911=CARTESIAN_POINT('Origin',(0.,0.,0.));
#22912=CARTESIAN_POINT('Origin',(0.,15.5739080413363,-1.3010426069826E-15));
#22913=CARTESIAN_POINT('',(0.,0.,0.));
#22914=CARTESIAN_POINT('Origin',(0.,0.,-25.0375057290932));
#22915=CARTESIAN_POINT('',(-7.9375,-9.72063396823212E-16,-14.1986));
#22916=CARTESIAN_POINT('Origin',(0.,0.,-14.1986));
#22917=CARTESIAN_POINT('',(-7.9375,-9.72063396823212E-16,-14.1732));
#22918=CARTESIAN_POINT('',(-7.9375,-9.72063396823212E-16,-25.0375057290932));
#22919=CARTESIAN_POINT('',(7.9375,9.72063396823212E-16,-14.1732));
#22920=CARTESIAN_POINT('Origin',(0.,0.,-14.1732));
#22921=CARTESIAN_POINT('Origin',(0.,0.,-14.1732));
#22922=CARTESIAN_POINT('Origin',(0.,0.,-14.1732));
#22923=CARTESIAN_POINT('',(-7.34187,8.99119759525598E-16,-13.7561353840161));
#22924=CARTESIAN_POINT('',(7.34187,-8.99119759525598E-16,-13.7561353840161));
#22925=CARTESIAN_POINT('Origin',(0.,0.,-13.7561353840161));
#22926=CARTESIAN_POINT('',(7.9375,-9.72063396823212E-16,-14.1732));
#22927=CARTESIAN_POINT('Origin',(0.,0.,-13.7561353840161));
#22928=CARTESIAN_POINT('Origin',(0.,0.,-0.45877107758224));
#22929=CARTESIAN_POINT('',(-7.34187,-8.99119759525598E-16,-0.417064615983855));
#22930=CARTESIAN_POINT('Origin',(0.,0.,-0.417064615983854));
#22931=CARTESIAN_POINT('',(-7.9375,-9.72063396823212E-16,3.60822483003176E-15));
#22932=CARTESIAN_POINT('',(-7.282307,-8.91825395795836E-16,-0.45877107758224));
#22933=CARTESIAN_POINT('Origin',(0.,0.,3.46944695195361E-15));
#22934=CARTESIAN_POINT('Origin',(0.,0.,-14.1986));
#22935=CARTESIAN_POINT('',(-7.34187,-8.99119759525598E-16,-14.1986));
#22936=CARTESIAN_POINT('Origin',(4.13777825740845E-15,13.7554856334967,
-14.1986));
#22937=CARTESIAN_POINT('',(-11.9126,6.87774281674836,-12.6111));
#22938=CARTESIAN_POINT('',(-11.9126,6.87774281674833,-1.58749999999999));
#22939=CARTESIAN_POINT('',(-11.9126,6.87774281674833,-14.1986));
#22940=CARTESIAN_POINT('',(-5.95630000000001,10.3166142251225,0.));
#22941=CARTESIAN_POINT('Ctrl Pts',(-11.9125999999999,6.87774281674839,-1.58749999999993));
#22942=CARTESIAN_POINT('Ctrl Pts',(-8.72062845024497,8.72062845024502,6.66133814775094E-15));
#22943=CARTESIAN_POINT('Ctrl Pts',(-5.95630000000001,10.3166142251225,5.86830536273203E-15));
#22944=CARTESIAN_POINT('',(1.04083408558608E-14,13.7554856334967,-1.5875));
#22945=CARTESIAN_POINT('Ctrl Pts',(-5.95630000000001,10.3166142251225,5.86830536273203E-15));
#22946=CARTESIAN_POINT('Ctrl Pts',(-3.19197154975503,11.9126,4.18737605265003E-15));
#22947=CARTESIAN_POINT('Ctrl Pts',(-8.46627770245953E-14,13.7554856334966,
-1.58749999999995));
#22948=CARTESIAN_POINT('',(1.04083408558608E-14,13.7554856334967,-12.6111));
#22949=CARTESIAN_POINT('',(4.13777825740845E-15,13.7554856334967,-14.1986));
#22950=CARTESIAN_POINT('',(-5.95630000000001,10.3166142251225,-14.1986));
#22951=CARTESIAN_POINT('Ctrl Pts',(-5.9563,10.3166142251225,-14.1986));
#22952=CARTESIAN_POINT('Ctrl Pts',(-3.19197154975503,11.9126,-14.1986));
#22953=CARTESIAN_POINT('Ctrl Pts',(-9.78569760414152E-14,13.7554856334966,
-12.6111));
#22954=CARTESIAN_POINT('Ctrl Pts',(-11.9125999999999,6.87774281674841,-12.6111000000001));
#22955=CARTESIAN_POINT('Ctrl Pts',(-8.72062845024495,8.72062845024504,-14.1986));
#22956=CARTESIAN_POINT('Ctrl Pts',(-5.9563,10.3166142251225,-14.1986));
#22957=CARTESIAN_POINT('Origin',(11.9126,6.87774281674832,-14.1986));
#22958=CARTESIAN_POINT('',(5.95630000000002,10.3166142251225,0.));
#22959=CARTESIAN_POINT('Ctrl Pts',(1.20946824320851E-13,13.7554856334966,
-1.58749999999994));
#22960=CARTESIAN_POINT('Ctrl Pts',(3.19197154975505,11.9126,-5.32907051820075E-15));
#22961=CARTESIAN_POINT('Ctrl Pts',(5.95630000000001,10.3166142251225,-3.06172453707759E-15));
#22962=CARTESIAN_POINT('',(11.9126,6.87774281674836,-1.5875));
#22963=CARTESIAN_POINT('Ctrl Pts',(5.95630000000001,10.3166142251225,-3.06172453707759E-15));
#22964=CARTESIAN_POINT('Ctrl Pts',(8.72062845024497,8.72062845024502,-1.80400037842164E-15));
#22965=CARTESIAN_POINT('Ctrl Pts',(11.9125999999999,6.87774281674839,-1.58749999999993));
#22966=CARTESIAN_POINT('',(11.9126,6.87774281674836,-12.6111));
#22967=CARTESIAN_POINT('',(11.9126,6.87774281674832,-14.1986));
#22968=CARTESIAN_POINT('',(5.95630000000002,10.3166142251225,-14.1986));
#22969=CARTESIAN_POINT('Ctrl Pts',(5.95630000000004,10.3166142251225,-14.1986));
#22970=CARTESIAN_POINT('Ctrl Pts',(8.72062845024499,8.72062845024502,-14.1986));
#22971=CARTESIAN_POINT('Ctrl Pts',(11.9125999999999,6.87774281674839,-12.6111000000001));
#22972=CARTESIAN_POINT('Ctrl Pts',(1.12700449935338E-13,13.7554856334966,
-12.6111000000001));
#22973=CARTESIAN_POINT('Ctrl Pts',(3.19197154975506,11.9126,-14.1986));
#22974=CARTESIAN_POINT('Ctrl Pts',(5.95630000000004,10.3166142251225,-14.1986));
#22975=CARTESIAN_POINT('Origin',(11.9126,6.87774281674832,-14.1986));
#22976=CARTESIAN_POINT('',(11.9126,-6.87774281674836,-1.5875));
#22977=CARTESIAN_POINT('',(11.9126,0.,0.));
#22978=CARTESIAN_POINT('Ctrl Pts',(11.9126,-6.87774281674825,-1.58749999999996));
#22979=CARTESIAN_POINT('Ctrl Pts',(11.9126,-3.19197154975496,-1.55431223447522E-15));
#22980=CARTESIAN_POINT('Ctrl Pts',(11.9126,-6.12344907415516E-15,-1.81290510726578E-30));
#22981=CARTESIAN_POINT('',(11.9126,-6.87774281674836,-12.6111));
#22982=CARTESIAN_POINT('',(11.9126,-6.87774281674836,-14.1986));
#22983=CARTESIAN_POINT('',(11.9126,0.,-14.1986));
#22984=CARTESIAN_POINT('Ctrl Pts',(11.9126,-6.87774281674825,-12.6111));
#22985=CARTESIAN_POINT('Ctrl Pts',(11.9126,-3.19197154975496,-14.1986));
#22986=CARTESIAN_POINT('Ctrl Pts',(11.9126,6.12344907415516E-15,-14.1986));
#22987=CARTESIAN_POINT('Ctrl Pts',(11.9126,6.12344907415516E-15,-14.1986));
#22988=CARTESIAN_POINT('Ctrl Pts',(11.9126,3.19197154975495,-14.1986));
#22989=CARTESIAN_POINT('Ctrl Pts',(11.9126,6.87774281674823,-12.6111000000001));
#22990=CARTESIAN_POINT('Ctrl Pts',(11.9126,-6.12344907415516E-15,1.53086226853879E-15));
#22991=CARTESIAN_POINT('Ctrl Pts',(11.9126,3.19197154975495,2.72627184089894E-15));
#22992=CARTESIAN_POINT('Ctrl Pts',(11.9126,6.87774281674825,-1.58749999999996));
#22993=CARTESIAN_POINT('Origin',(-1.00154306582478E-15,-13.7554856334967,
-14.1986));
#22994=CARTESIAN_POINT('',(5.95630000000001,-10.3166142251225,0.));
#22995=CARTESIAN_POINT('Ctrl Pts',(11.9125999999999,-6.87774281674842,-1.58749999999994));
#22996=CARTESIAN_POINT('Ctrl Pts',(8.72062845024498,-8.72062845024505,-1.93178806284777E-14));
#22997=CARTESIAN_POINT('Ctrl Pts',(5.95630000000004,-10.3166142251225,-1.70946286653499E-14));
#22998=CARTESIAN_POINT('',(-5.29090660172926E-14,-13.7554856334967,-1.5875));
#22999=CARTESIAN_POINT('Ctrl Pts',(5.95630000000004,-10.3166142251225,-1.70946286653499E-14));
#23000=CARTESIAN_POINT('Ctrl Pts',(3.19197154975504,-11.9126,-1.44505874102389E-14));
#23001=CARTESIAN_POINT('Ctrl Pts',(6.92695448383054E-14,-13.7554856334967,
-1.58749999999999));
#23002=CARTESIAN_POINT('',(-5.29090660172926E-14,-13.7554856334967,-12.6111));
#23003=CARTESIAN_POINT('',(-1.00154306582478E-15,-13.7554856334967,-14.1986));
#23004=CARTESIAN_POINT('',(5.95630000000001,-10.3166142251225,-14.1986));
#23005=CARTESIAN_POINT('Ctrl Pts',(5.95630000000002,-10.3166142251225,-14.1986));
#23006=CARTESIAN_POINT('Ctrl Pts',(3.19197154975504,-11.9126,-14.1986));
#23007=CARTESIAN_POINT('Ctrl Pts',(9.5108184579578E-14,-13.7554856334967,
-12.6111));
#23008=CARTESIAN_POINT('Ctrl Pts',(11.9125999999999,-6.87774281674842,-12.6111));
#23009=CARTESIAN_POINT('Ctrl Pts',(8.72062845024498,-8.72062845024506,-14.1986));
#23010=CARTESIAN_POINT('Ctrl Pts',(5.95630000000002,-10.3166142251225,-14.1986));
#23011=CARTESIAN_POINT('Origin',(-11.9126,-6.87774281674836,-14.1986));
#23012=CARTESIAN_POINT('',(-5.95630000000001,-10.3166142251225,0.));
#23013=CARTESIAN_POINT('Ctrl Pts',(-1.53382563570533E-13,-13.7554856334966,
-1.58749999999994));
#23014=CARTESIAN_POINT('Ctrl Pts',(-3.19197154975508,-11.9126,-1.11022302462516E-14));
#23015=CARTESIAN_POINT('Ctrl Pts',(-5.95630000000005,-10.3166142251225,
-1.7349772376773E-14));
#23016=CARTESIAN_POINT('',(-11.9126,-6.87774281674836,-1.5875));
#23017=CARTESIAN_POINT('Ctrl Pts',(-5.95630000000005,-10.3166142251225,
-1.7349772376773E-14));
#23018=CARTESIAN_POINT('Ctrl Pts',(-8.720628450245,-8.72062845024504,-2.3722279033548E-14));
#23019=CARTESIAN_POINT('Ctrl Pts',(-11.9125999999999,-6.87774281674841,
-1.58749999999995));
#23020=CARTESIAN_POINT('',(-11.9126,-6.87774281674836,-12.6111));
#23021=CARTESIAN_POINT('',(-11.9126,-6.87774281674836,-14.1986));
#23022=CARTESIAN_POINT('',(-5.95630000000001,-10.3166142251225,-14.1986));
#23023=CARTESIAN_POINT('Ctrl Pts',(-5.95630000000004,-10.3166142251225,
-14.1986));
#23024=CARTESIAN_POINT('Ctrl Pts',(-8.72062845024499,-8.72062845024504,
-14.1986));
#23025=CARTESIAN_POINT('Ctrl Pts',(-11.9125999999999,-6.87774281674841,
-12.6111000000001));
#23026=CARTESIAN_POINT('Ctrl Pts',(-1.66576762587353E-13,-13.7554856334966,
-12.6111000000001));
#23027=CARTESIAN_POINT('Ctrl Pts',(-3.19197154975508,-11.9126,-14.1986));
#23028=CARTESIAN_POINT('Ctrl Pts',(-5.95630000000004,-10.3166142251225,
-14.1986));
#23029=CARTESIAN_POINT('Origin',(-11.9126,6.87774281674833,-14.1986));
#23030=CARTESIAN_POINT('',(-11.9126,1.50231459873716E-15,0.));
#23031=CARTESIAN_POINT('Ctrl Pts',(-11.9126,-6.87774281674822,-1.58749999999994));
#23032=CARTESIAN_POINT('Ctrl Pts',(-11.9126,-3.19197154975494,2.44249065417534E-15));
#23033=CARTESIAN_POINT('Ctrl Pts',(-11.9126,6.12344907415516E-15,5.10287422846262E-16));
#23034=CARTESIAN_POINT('Ctrl Pts',(-11.9126,6.12344907415516E-15,5.10287422846262E-16));
#23035=CARTESIAN_POINT('Ctrl Pts',(-11.9126,3.19197154975495,-7.93896261275937E-16));
#23036=CARTESIAN_POINT('Ctrl Pts',(-11.9126,6.87774281674822,-1.58749999999994));
#23037=CARTESIAN_POINT('',(-11.9126,1.50231459873716E-15,-14.1986));
#23038=CARTESIAN_POINT('Ctrl Pts',(-11.9126,2.04114969138505E-14,-14.1986));
#23039=CARTESIAN_POINT('Ctrl Pts',(-11.9126,3.19197154975496,-14.1986));
#23040=CARTESIAN_POINT('Ctrl Pts',(-11.9126,6.87774281674823,-12.6111000000001));
#23041=CARTESIAN_POINT('Ctrl Pts',(-11.9126,-6.87774281674826,-12.6111));
#23042=CARTESIAN_POINT('Ctrl Pts',(-11.9126,-3.19197154975495,-14.1986));
#23043=CARTESIAN_POINT('Ctrl Pts',(-11.9126,2.04114969138505E-14,-14.1986));
#23044=CARTESIAN_POINT('Origin',(5.20417042793042E-15,13.7554856334967,
0.));
#23045=CARTESIAN_POINT('Origin',(0.,0.,0.));
#23046=CARTESIAN_POINT('Origin',(0.,0.,0.));
#23047=CARTESIAN_POINT('Origin',(0.,0.,0.));
#23048=CARTESIAN_POINT('Origin',(0.,0.,0.));
#23049=CARTESIAN_POINT('Origin',(0.,0.,0.));
#23050=CARTESIAN_POINT('Origin',(0.,0.,0.));
#23051=CARTESIAN_POINT('Origin',(5.20417042793042E-15,13.7554856334967,
-14.1986));
#23052=CARTESIAN_POINT('Origin',(0.,0.,-14.1986));
#23053=CARTESIAN_POINT('Origin',(0.,0.,-14.1986));
#23054=CARTESIAN_POINT('Origin',(0.,0.,-14.1986));
#23055=CARTESIAN_POINT('Origin',(0.,0.,-14.1986));
#23056=CARTESIAN_POINT('Origin',(0.,0.,-14.1986));
#23057=CARTESIAN_POINT('Origin',(0.,0.,-14.1986));
#23058=CARTESIAN_POINT('Origin',(0.,0.,-14.1986));
#23059=CARTESIAN_POINT('Origin',(0.,0.,-14.1986));
#23060=CARTESIAN_POINT('Origin',(0.,0.,-14.1986));
#23061=CARTESIAN_POINT('Origin',(0.,0.,-14.1986));
#23062=CARTESIAN_POINT('Origin',(0.,0.,-14.1986));
#23063=CARTESIAN_POINT('Origin',(0.,0.,-14.1986));
#23064=CARTESIAN_POINT('Origin',(0.,0.,0.));
#23065=CARTESIAN_POINT('Origin',(0.,0.,0.));
#23066=CARTESIAN_POINT('Origin',(0.,0.,0.));
#23067=CARTESIAN_POINT('Origin',(0.,0.,0.));
#23068=CARTESIAN_POINT('Origin',(0.,0.,0.));
#23069=CARTESIAN_POINT('Origin',(0.,0.,0.));
#23070=CARTESIAN_POINT('',(0.,0.,0.));
#23071=CARTESIAN_POINT('Origin',(-2.53888687851145E-9,74.888750003468,-7.9374999999999));
#23072=CARTESIAN_POINT('',(6.5626846775001,73.3012500034686,-7.93750000000257));
#23073=CARTESIAN_POINT('',(6.5626846775001,73.9362500034686,-7.9375000000015));
#23074=CARTESIAN_POINT('',(6.56268467242224,74.8887500034674,-7.93749999999981));
#23075=CARTESIAN_POINT('',(-5.80913668152327,74.3748153225002,-10.9908197002073));
#23076=CARTESIAN_POINT('Ctrl Pts',(-5.80913668152327,74.3748153225002,-10.9908197002073));
#23077=CARTESIAN_POINT('Ctrl Pts',(-5.58830892045767,74.3455189140323,-11.4109586876241));
#23078=CARTESIAN_POINT('Ctrl Pts',(-5.30932343282159,74.3172500034687,-11.7949492688802));
#23079=CARTESIAN_POINT('Ctrl Pts',(-4.05596218814306,74.1902500034686,-13.5200530258749));
#23080=CARTESIAN_POINT('Ctrl Pts',(-2.02798109407148,74.0632500034687,-14.1789840269267));
#23081=CARTESIAN_POINT('Ctrl Pts',(1.1673575708729E-13,73.9362500034686,
-14.8379150279786));
#23082=CARTESIAN_POINT('Ctrl Pts',(2.0279810940716,73.8092500034687,-14.1789840269267));
#23083=CARTESIAN_POINT('Ctrl Pts',(4.05596218814324,73.6822500034687,-13.5200530258749));
#23084=CARTESIAN_POINT('Ctrl Pts',(5.30932343282159,73.5552500034686,-11.7949492688802));
#23085=CARTESIAN_POINT('Ctrl Pts',(6.56268467750003,73.4282500034686,-10.0698455118856));
#23086=CARTESIAN_POINT('Ctrl Pts',(6.5626846775001,73.3012500034686,-7.93749999999999));
#23087=CARTESIAN_POINT('',(3.07575458830291,74.3748153227072,-13.7347893553626));
#23088=CARTESIAN_POINT('Origin',(2.12052597703405E-13,74.3748153225018,
-7.93750000000196));
#23089=CARTESIAN_POINT('Ctrl Pts',(3.07575458898229,74.3748153225002,-13.7347893566431));
#23090=CARTESIAN_POINT('Ctrl Pts',(4.41692449403691,74.2806745843362,-13.0232310340711));
#23091=CARTESIAN_POINT('Ctrl Pts',(5.30932343282159,74.1902500034686,-11.7949492688802));
#23092=CARTESIAN_POINT('Ctrl Pts',(6.56268467750008,74.0632500034686,-10.0698455118856));
#23093=CARTESIAN_POINT('Ctrl Pts',(6.5626846775001,73.9362500034686,-7.93749999999999));
#23094=CARTESIAN_POINT('Origin',(-2.53888687851145E-9,74.888750003468,-7.9374999999999));
#23095=CARTESIAN_POINT('',(6.56268467749999,70.7612500034687,-7.93750000000685));
#23096=CARTESIAN_POINT('',(6.5626846775001,71.3962500034686,-7.93750000000578));
#23097=CARTESIAN_POINT('',(6.56268467242224,74.8887500034674,-7.93749999999981));
#23098=CARTESIAN_POINT('Ctrl Pts',(6.5626846775001,73.3012500034686,-7.93749999999999));
#23099=CARTESIAN_POINT('Ctrl Pts',(6.56268467750003,73.1742500034686,-5.80515448811441));
#23100=CARTESIAN_POINT('Ctrl Pts',(5.30932343282164,73.0472500034686,-4.08005073111967));
#23101=CARTESIAN_POINT('Ctrl Pts',(4.05596218814318,72.9202500034686,-2.35494697412514));
#23102=CARTESIAN_POINT('Ctrl Pts',(2.02798109407154,72.7932500034686,-1.69601597307328));
#23103=CARTESIAN_POINT('Ctrl Pts',(1.1673575708729E-13,72.6662500034686,
-1.0370849720215));
#23104=CARTESIAN_POINT('Ctrl Pts',(-2.02798109407165,72.5392500034687,-1.69601597307328));
#23105=CARTESIAN_POINT('Ctrl Pts',(-4.05596218814312,72.4122500034686,-2.35494697412514));
#23106=CARTESIAN_POINT('Ctrl Pts',(-5.30932343282153,72.2852500034685,-4.08005073111967));
#23107=CARTESIAN_POINT('Ctrl Pts',(-6.56268467750008,72.1582500034687,-5.80515448811441));
#23108=CARTESIAN_POINT('Ctrl Pts',(-6.56268467750004,72.0312500034686,-7.93749999999999));
#23109=CARTESIAN_POINT('Ctrl Pts',(-6.56268467750003,71.9042500034686,-10.0698455118856));
#23110=CARTESIAN_POINT('Ctrl Pts',(-5.30932343282159,71.7772500034686,-11.7949492688802));
#23111=CARTESIAN_POINT('Ctrl Pts',(-4.05596218814318,71.6502500034686,-13.5200530258749));
#23112=CARTESIAN_POINT('Ctrl Pts',(-2.0279810940716,71.5232500034686,-14.1789840269267));
#23113=CARTESIAN_POINT('Ctrl Pts',(0.,71.3962500034686,-14.8379150279786));
#23114=CARTESIAN_POINT('Ctrl Pts',(2.02798109407165,71.2692500034687,-14.1789840269267));
#23115=CARTESIAN_POINT('Ctrl Pts',(4.05596218814312,71.1422500034685,-13.5200530258749));
#23116=CARTESIAN_POINT('Ctrl Pts',(5.30932343282159,71.0152500034686,-11.7949492688802));
#23117=CARTESIAN_POINT('Ctrl Pts',(6.56268467750003,70.8882500034686,-10.0698455118856));
#23118=CARTESIAN_POINT('Ctrl Pts',(6.56268467749999,70.7612500034687,-7.93749999999999));
#23119=CARTESIAN_POINT('Ctrl Pts',(6.5626846775001,73.9362500034686,-7.93749999999999));
#23120=CARTESIAN_POINT('Ctrl Pts',(6.56268467749991,73.8092500034686,-5.80515448811441));
#23121=CARTESIAN_POINT('Ctrl Pts',(5.30932343282159,73.6822500034686,-4.08005073111967));
#23122=CARTESIAN_POINT('Ctrl Pts',(4.05596218814324,73.5552500034685,-2.35494697412514));
#23123=CARTESIAN_POINT('Ctrl Pts',(2.02798109407165,73.4282500034686,-1.69601597307328));
#23124=CARTESIAN_POINT('Ctrl Pts',(0.,73.3012500034685,-1.0370849720215));
#23125=CARTESIAN_POINT('Ctrl Pts',(-2.02798109407154,73.1742500034685,-1.69601597307328));
#23126=CARTESIAN_POINT('Ctrl Pts',(-4.05596218814312,73.0472500034687,-2.35494697412514));
#23127=CARTESIAN_POINT('Ctrl Pts',(-5.30932343282159,72.9202500034686,-4.08005073111967));
#23128=CARTESIAN_POINT('Ctrl Pts',(-6.56268467750003,72.7932500034685,-5.80515448811441));
#23129=CARTESIAN_POINT('Ctrl Pts',(-6.56268467749993,72.6662500034687,-7.93749999999999));
#23130=CARTESIAN_POINT('Ctrl Pts',(-6.56268467749997,72.5392500034685,-10.0698455118856));
#23131=CARTESIAN_POINT('Ctrl Pts',(-5.30932343282159,72.4122500034687,-11.7949492688802));
#23132=CARTESIAN_POINT('Ctrl Pts',(-4.05596218814312,72.2852500034686,-13.5200530258749));
#23133=CARTESIAN_POINT('Ctrl Pts',(-2.0279810940716,72.1582500034688,-14.1789840269267));
#23134=CARTESIAN_POINT('Ctrl Pts',(0.,72.0312500034686,-14.8379150279786));
#23135=CARTESIAN_POINT('Ctrl Pts',(2.02798109407154,71.9042500034687,-14.1789840269267));
#23136=CARTESIAN_POINT('Ctrl Pts',(4.05596218814318,71.7772500034686,-13.5200530258749));
#23137=CARTESIAN_POINT('Ctrl Pts',(5.30932343282159,71.6502500034686,-11.7949492688802));
#23138=CARTESIAN_POINT('Ctrl Pts',(6.56268467750003,71.5232500034685,-10.0698455118856));
#23139=CARTESIAN_POINT('Ctrl Pts',(6.5626846775001,71.3962500034686,-7.93749999999999));
#23140=CARTESIAN_POINT('Origin',(-2.53888687851145E-9,74.888750003468,-7.9374999999999));
#23141=CARTESIAN_POINT('',(6.56268467749999,68.2212500034686,-7.93750000001112));
#23142=CARTESIAN_POINT('',(6.56268467749999,68.8562500034686,-7.93750000001005));
#23143=CARTESIAN_POINT('',(6.56268467242224,74.8887500034674,-7.93749999999981));
#23144=CARTESIAN_POINT('Ctrl Pts',(6.56268467749999,70.7612500034687,-7.93749999999999));
#23145=CARTESIAN_POINT('Ctrl Pts',(6.56268467750003,70.6342500034686,-5.80515448811441));
#23146=CARTESIAN_POINT('Ctrl Pts',(5.30932343282164,70.5072500034686,-4.08005073111967));
#23147=CARTESIAN_POINT('Ctrl Pts',(4.05596218814324,70.3802500034686,-2.35494697412514));
#23148=CARTESIAN_POINT('Ctrl Pts',(2.0279810940716,70.2532500034686,-1.69601597307328));
#23149=CARTESIAN_POINT('Ctrl Pts',(0.,70.1262500034686,-1.0370849720215));
#23150=CARTESIAN_POINT('Ctrl Pts',(-2.0279810940716,69.9992500034686,-1.69601597307328));
#23151=CARTESIAN_POINT('Ctrl Pts',(-4.05596218814312,69.8722500034686,-2.35494697412514));
#23152=CARTESIAN_POINT('Ctrl Pts',(-5.30932343282159,69.7452500034687,-4.08005073111967));
#23153=CARTESIAN_POINT('Ctrl Pts',(-6.56268467749997,69.6182500034686,-5.80515448811441));
#23154=CARTESIAN_POINT('Ctrl Pts',(-6.56268467749999,69.4912500034686,-7.93749999999999));
#23155=CARTESIAN_POINT('Ctrl Pts',(-6.56268467749997,69.3642500034686,-10.0698455118856));
#23156=CARTESIAN_POINT('Ctrl Pts',(-5.30932343282153,69.2372500034686,-11.7949492688802));
#23157=CARTESIAN_POINT('Ctrl Pts',(-4.05596218814312,69.1102500034686,-13.5200530258749));
#23158=CARTESIAN_POINT('Ctrl Pts',(-2.02798109407154,68.9832500034687,-14.1789840269267));
#23159=CARTESIAN_POINT('Ctrl Pts',(0.,68.8562500034685,-14.8379150279786));
#23160=CARTESIAN_POINT('Ctrl Pts',(2.02798109407165,68.7292500034686,-14.1789840269267));
#23161=CARTESIAN_POINT('Ctrl Pts',(4.05596218814312,68.6022500034686,-13.5200530258749));
#23162=CARTESIAN_POINT('Ctrl Pts',(5.30932343282164,68.4752500034687,-11.7949492688802));
#23163=CARTESIAN_POINT('Ctrl Pts',(6.56268467749997,68.3482500034685,-10.0698455118856));
#23164=CARTESIAN_POINT('Ctrl Pts',(6.56268467749999,68.2212500034686,-7.93749999999999));
#23165=CARTESIAN_POINT('Ctrl Pts',(6.5626846775001,71.3962500034686,-7.93749999999999));
#23166=CARTESIAN_POINT('Ctrl Pts',(6.56268467750008,71.2692500034686,-5.80515448811441));
#23167=CARTESIAN_POINT('Ctrl Pts',(5.30932343282153,71.1422500034686,-4.08005073111967));
#23168=CARTESIAN_POINT('Ctrl Pts',(4.05596218814312,71.0152500034686,-2.35494697412514));
#23169=CARTESIAN_POINT('Ctrl Pts',(2.0279810940716,70.8882500034687,-1.69601597307328));
#23170=CARTESIAN_POINT('Ctrl Pts',(0.,70.7612500034686,-1.0370849720215));
#23171=CARTESIAN_POINT('Ctrl Pts',(-2.02798109407148,70.6342500034686,-1.69601597307328));
#23172=CARTESIAN_POINT('Ctrl Pts',(-4.05596218814318,70.5072500034686,-2.35494697412514));
#23173=CARTESIAN_POINT('Ctrl Pts',(-5.30932343282159,70.3802500034686,-4.08005073111967));
#23174=CARTESIAN_POINT('Ctrl Pts',(-6.56268467750003,70.2532500034686,-5.80515448811441));
#23175=CARTESIAN_POINT('Ctrl Pts',(-6.56268467749999,70.1262500034686,-7.93749999999999));
#23176=CARTESIAN_POINT('Ctrl Pts',(-6.56268467750003,69.9992500034686,-10.0698455118856));
#23177=CARTESIAN_POINT('Ctrl Pts',(-5.30932343282153,69.8722500034687,-11.7949492688802));
#23178=CARTESIAN_POINT('Ctrl Pts',(-4.05596218814324,69.7452500034685,-13.5200530258749));
#23179=CARTESIAN_POINT('Ctrl Pts',(-2.02798109407154,69.6182500034687,-14.1789840269267));
#23180=CARTESIAN_POINT('Ctrl Pts',(-5.83678785436452E-14,69.4912500034686,
-14.8379150279786));
#23181=CARTESIAN_POINT('Ctrl Pts',(2.02798109407154,69.3642500034687,-14.1789840269267));
#23182=CARTESIAN_POINT('Ctrl Pts',(4.05596218814318,69.2372500034687,-13.5200530258749));
#23183=CARTESIAN_POINT('Ctrl Pts',(5.30932343282164,69.1102500034686,-11.7949492688802));
#23184=CARTESIAN_POINT('Ctrl Pts',(6.56268467750003,68.9832500034685,-10.0698455118856));
#23185=CARTESIAN_POINT('Ctrl Pts',(6.56268467749999,68.8562500034686,-7.93749999999999));
#23186=CARTESIAN_POINT('Origin',(-2.53888687851145E-9,74.888750003468,-7.9374999999999));
#23187=CARTESIAN_POINT('',(6.56268467749999,65.6812500034686,-7.9375000000154));
#23188=CARTESIAN_POINT('',(6.56268467749999,66.3162500034687,-7.93750000001433));
#23189=CARTESIAN_POINT('',(6.56268467242224,74.8887500034674,-7.93749999999981));
#23190=CARTESIAN_POINT('Ctrl Pts',(6.56268467749999,68.2212500034686,-7.93749999999999));
#23191=CARTESIAN_POINT('Ctrl Pts',(6.56268467750003,68.0942500034685,-5.80515448811441));
#23192=CARTESIAN_POINT('Ctrl Pts',(5.3093234328217,67.9672500034686,-4.08005073111967));
#23193=CARTESIAN_POINT('Ctrl Pts',(4.05596218814312,67.8402500034685,-2.35494697412514));
#23194=CARTESIAN_POINT('Ctrl Pts',(2.0279810940716,67.7132500034686,-1.69601597307328));
#23195=CARTESIAN_POINT('Ctrl Pts',(1.1673575708729E-13,67.5862500034685,
-1.0370849720215));
#23196=CARTESIAN_POINT('Ctrl Pts',(-2.0279810940716,67.4592500034686,-1.69601597307328));
#23197=CARTESIAN_POINT('Ctrl Pts',(-4.05596218814312,67.3322500034685,-2.35494697412514));
#23198=CARTESIAN_POINT('Ctrl Pts',(-5.30932343282153,67.2052500034686,-4.08005073111967));
#23199=CARTESIAN_POINT('Ctrl Pts',(-6.56268467750003,67.0782500034685,-5.80515448811441));
#23200=CARTESIAN_POINT('Ctrl Pts',(-6.56268467749999,66.9512500034686,-7.93749999999999));
#23201=CARTESIAN_POINT('Ctrl Pts',(-6.56268467749997,66.8242500034685,-10.0698455118856));
#23202=CARTESIAN_POINT('Ctrl Pts',(-5.30932343282153,66.6972500034686,-11.7949492688802));
#23203=CARTESIAN_POINT('Ctrl Pts',(-4.05596218814312,66.5702500034686,-13.5200530258749));
#23204=CARTESIAN_POINT('Ctrl Pts',(-2.02798109407165,66.4432500034688,-14.1789840269267));
#23205=CARTESIAN_POINT('Ctrl Pts',(0.,66.3162500034685,-14.8379150279786));
#23206=CARTESIAN_POINT('Ctrl Pts',(2.02798109407154,66.1892500034688,-14.1789840269267));
#23207=CARTESIAN_POINT('Ctrl Pts',(4.05596218814312,66.0622500034686,-13.5200530258749));
#23208=CARTESIAN_POINT('Ctrl Pts',(5.30932343282164,65.9352500034686,-11.7949492688802));
#23209=CARTESIAN_POINT('Ctrl Pts',(6.56268467750008,65.8082500034686,-10.0698455118856));
#23210=CARTESIAN_POINT('Ctrl Pts',(6.56268467749999,65.6812500034686,-7.93749999999999));
#23211=CARTESIAN_POINT('Ctrl Pts',(6.56268467749999,68.8562500034686,-7.93749999999999));
#23212=CARTESIAN_POINT('Ctrl Pts',(6.56268467750003,68.7292500034685,-5.80515448811441));
#23213=CARTESIAN_POINT('Ctrl Pts',(5.30932343282159,68.6022500034686,-4.08005073111967));
#23214=CARTESIAN_POINT('Ctrl Pts',(4.05596218814318,68.4752500034685,-2.35494697412514));
#23215=CARTESIAN_POINT('Ctrl Pts',(2.0279810940716,68.3482500034686,-1.69601597307328));
#23216=CARTESIAN_POINT('Ctrl Pts',(-1.1673575708729E-13,68.2212500034685,
-1.0370849720215));
#23217=CARTESIAN_POINT('Ctrl Pts',(-2.02798109407154,68.0942500034687,-1.69601597307328));
#23218=CARTESIAN_POINT('Ctrl Pts',(-4.05596218814306,67.9672500034686,-2.35494697412514));
#23219=CARTESIAN_POINT('Ctrl Pts',(-5.30932343282159,67.8402500034686,-4.08005073111967));
#23220=CARTESIAN_POINT('Ctrl Pts',(-6.56268467749997,67.7132500034685,-5.80515448811441));
#23221=CARTESIAN_POINT('Ctrl Pts',(-6.56268467749999,67.5862500034686,-7.93749999999999));
#23222=CARTESIAN_POINT('Ctrl Pts',(-6.56268467749991,67.4592500034685,-10.0698455118856));
#23223=CARTESIAN_POINT('Ctrl Pts',(-5.30932343282153,67.3322500034686,-11.7949492688802));
#23224=CARTESIAN_POINT('Ctrl Pts',(-4.05596218814312,67.2052500034686,-13.5200530258749));
#23225=CARTESIAN_POINT('Ctrl Pts',(-2.02798109407154,67.0782500034687,-14.1789840269267));
#23226=CARTESIAN_POINT('Ctrl Pts',(0.,66.9512500034685,-14.8379150279786));
#23227=CARTESIAN_POINT('Ctrl Pts',(2.02798109407154,66.8242500034687,-14.1789840269267));
#23228=CARTESIAN_POINT('Ctrl Pts',(4.05596218814318,66.6972500034686,-13.5200530258749));
#23229=CARTESIAN_POINT('Ctrl Pts',(5.30932343282153,66.5702500034686,-11.7949492688802));
#23230=CARTESIAN_POINT('Ctrl Pts',(6.56268467750003,66.4432500034685,-10.0698455118856));
#23231=CARTESIAN_POINT('Ctrl Pts',(6.56268467749999,66.3162500034687,-7.93749999999999));
#23232=CARTESIAN_POINT('Origin',(-2.53888687851145E-9,74.888750003468,-7.9374999999999));
#23233=CARTESIAN_POINT('',(6.56268467750004,63.1412500034686,-7.93750000001967));
#23234=CARTESIAN_POINT('',(6.56268467749999,63.7762500034686,-7.9375000000186));
#23235=CARTESIAN_POINT('',(6.56268467242224,74.8887500034674,-7.93749999999981));
#23236=CARTESIAN_POINT('Ctrl Pts',(6.56268467749999,65.6812500034686,-7.93749999999999));
#23237=CARTESIAN_POINT('Ctrl Pts',(6.56268467749991,65.5542500034687,-5.80515448811441));
#23238=CARTESIAN_POINT('Ctrl Pts',(5.3093234328217,65.4272500034686,-4.08005073111967));
#23239=CARTESIAN_POINT('Ctrl Pts',(4.05596218814324,65.3002500034687,-2.35494697412514));
#23240=CARTESIAN_POINT('Ctrl Pts',(2.0279810940716,65.1732500034686,-1.69601597307328));
#23241=CARTESIAN_POINT('Ctrl Pts',(0.,65.0462500034686,-1.0370849720215));
#23242=CARTESIAN_POINT('Ctrl Pts',(-2.0279810940716,64.9192500034686,-1.69601597307328));
#23243=CARTESIAN_POINT('Ctrl Pts',(-4.05596218814312,64.7922500034686,-2.35494697412514));
#23244=CARTESIAN_POINT('Ctrl Pts',(-5.30932343282153,64.6652500034686,-4.08005073111967));
#23245=CARTESIAN_POINT('Ctrl Pts',(-6.56268467750003,64.5382500034686,-5.80515448811441));
#23246=CARTESIAN_POINT('Ctrl Pts',(-6.56268467749999,64.4112500034687,-7.93749999999999));
#23247=CARTESIAN_POINT('Ctrl Pts',(-6.56268467749997,64.2842500034685,-10.0698455118856));
#23248=CARTESIAN_POINT('Ctrl Pts',(-5.30932343282148,64.1572500034686,-11.7949492688802));
#23249=CARTESIAN_POINT('Ctrl Pts',(-4.05596218814312,64.0302500034686,-13.5200530258749));
#23250=CARTESIAN_POINT('Ctrl Pts',(-2.02798109407165,63.9032500034688,-14.1789840269267));
#23251=CARTESIAN_POINT('Ctrl Pts',(0.,63.7762500034686,-14.8379150279786));
#23252=CARTESIAN_POINT('Ctrl Pts',(2.0279810940716,63.6492500034688,-14.1789840269267));
#23253=CARTESIAN_POINT('Ctrl Pts',(4.05596218814312,63.5222500034685,-13.5200530258749));
#23254=CARTESIAN_POINT('Ctrl Pts',(5.3093234328217,63.3952500034686,-11.7949492688802));
#23255=CARTESIAN_POINT('Ctrl Pts',(6.56268467749997,63.2682500034685,-10.0698455118856));
#23256=CARTESIAN_POINT('Ctrl Pts',(6.56268467750004,63.1412500034686,-7.93749999999999));
#23257=CARTESIAN_POINT('Ctrl Pts',(6.56268467749999,66.3162500034687,-7.93749999999999));
#23258=CARTESIAN_POINT('Ctrl Pts',(6.56268467749997,66.1892500034686,-5.80515448811441));
#23259=CARTESIAN_POINT('Ctrl Pts',(5.30932343282159,66.0622500034686,-4.08005073111967));
#23260=CARTESIAN_POINT('Ctrl Pts',(4.05596218814318,65.9352500034686,-2.35494697412514));
#23261=CARTESIAN_POINT('Ctrl Pts',(2.02798109407148,65.8082500034686,-1.69601597307328));
#23262=CARTESIAN_POINT('Ctrl Pts',(5.83678785436452E-14,65.6812500034686,
-1.0370849720215));
#23263=CARTESIAN_POINT('Ctrl Pts',(-2.0279810940716,65.5542500034686,-1.69601597307328));
#23264=CARTESIAN_POINT('Ctrl Pts',(-4.05596218814318,65.4272500034686,-2.35494697412514));
#23265=CARTESIAN_POINT('Ctrl Pts',(-5.30932343282153,65.3002500034686,-4.08005073111967));
#23266=CARTESIAN_POINT('Ctrl Pts',(-6.56268467749997,65.1732500034685,-5.80515448811441));
#23267=CARTESIAN_POINT('Ctrl Pts',(-6.56268467749999,65.0462500034685,-7.93749999999999));
#23268=CARTESIAN_POINT('Ctrl Pts',(-6.56268467750003,64.9192500034685,-10.0698455118856));
#23269=CARTESIAN_POINT('Ctrl Pts',(-5.30932343282159,64.7922500034686,-11.7949492688802));
#23270=CARTESIAN_POINT('Ctrl Pts',(-4.05596218814306,64.6652500034686,-13.5200530258749));
#23271=CARTESIAN_POINT('Ctrl Pts',(-2.02798109407154,64.5382500034687,-14.1789840269267));
#23272=CARTESIAN_POINT('Ctrl Pts',(1.1673575708729E-13,64.4112500034686,
-14.8379150279786));
#23273=CARTESIAN_POINT('Ctrl Pts',(2.0279810940716,64.2842500034687,-14.1789840269267));
#23274=CARTESIAN_POINT('Ctrl Pts',(4.05596218814324,64.1572500034685,-13.5200530258749));
#23275=CARTESIAN_POINT('Ctrl Pts',(5.30932343282159,64.0302500034686,-11.7949492688802));
#23276=CARTESIAN_POINT('Ctrl Pts',(6.56268467750003,63.9032500034685,-10.0698455118856));
#23277=CARTESIAN_POINT('Ctrl Pts',(6.56268467749999,63.7762500034686,-7.93749999999999));
#23278=CARTESIAN_POINT('Origin',(-2.53888687851145E-9,74.888750003468,-7.9374999999999));
#23279=CARTESIAN_POINT('',(6.5626846775001,60.6012500034686,-7.93750000002395));
#23280=CARTESIAN_POINT('',(6.56268467749993,61.2362500034686,-7.93750000002288));
#23281=CARTESIAN_POINT('',(6.56268467242224,74.8887500034674,-7.93749999999981));
#23282=CARTESIAN_POINT('Ctrl Pts',(6.56268467750004,63.1412500034686,-7.93749999999999));
#23283=CARTESIAN_POINT('Ctrl Pts',(6.56268467750003,63.0142500034686,-5.80515448811441));
#23284=CARTESIAN_POINT('Ctrl Pts',(5.30932343282164,62.8872500034686,-4.08005073111967));
#23285=CARTESIAN_POINT('Ctrl Pts',(4.05596218814312,62.7602500034686,-2.35494697412514));
#23286=CARTESIAN_POINT('Ctrl Pts',(2.02798109407165,62.6332500034686,-1.69601597307328));
#23287=CARTESIAN_POINT('Ctrl Pts',(0.,62.5062500034686,-1.0370849720215));
#23288=CARTESIAN_POINT('Ctrl Pts',(-2.02798109407154,62.3792500034686,-1.69601597307328));
#23289=CARTESIAN_POINT('Ctrl Pts',(-4.05596218814324,62.2522500034685,-2.35494697412514));
#23290=CARTESIAN_POINT('Ctrl Pts',(-5.30932343282148,62.1252500034686,-4.08005073111967));
#23291=CARTESIAN_POINT('Ctrl Pts',(-6.56268467750003,61.9982500034685,-5.80515448811441));
#23292=CARTESIAN_POINT('Ctrl Pts',(-6.5626846775001,61.8712500034687,-7.93749999999999));
#23293=CARTESIAN_POINT('Ctrl Pts',(-6.56268467750008,61.7442500034686,-10.0698455118856));
#23294=CARTESIAN_POINT('Ctrl Pts',(-5.30932343282148,61.6172500034687,-11.7949492688802));
#23295=CARTESIAN_POINT('Ctrl Pts',(-4.05596218814312,61.4902500034686,-13.5200530258749));
#23296=CARTESIAN_POINT('Ctrl Pts',(-2.0279810940716,61.3632500034687,-14.1789840269267));
#23297=CARTESIAN_POINT('Ctrl Pts',(0.,61.2362500034686,-14.8379150279786));
#23298=CARTESIAN_POINT('Ctrl Pts',(2.0279810940716,61.1092500034687,-14.1789840269267));
#23299=CARTESIAN_POINT('Ctrl Pts',(4.05596218814318,60.9822500034686,-13.5200530258749));
#23300=CARTESIAN_POINT('Ctrl Pts',(5.3093234328217,60.8552500034686,-11.7949492688802));
#23301=CARTESIAN_POINT('Ctrl Pts',(6.56268467750003,60.7282500034687,-10.0698455118856));
#23302=CARTESIAN_POINT('Ctrl Pts',(6.5626846775001,60.6012500034686,-7.93749999999999));
#23303=CARTESIAN_POINT('Ctrl Pts',(6.56268467749999,63.7762500034686,-7.93749999999999));
#23304=CARTESIAN_POINT('Ctrl Pts',(6.56268467750008,63.6492500034686,-5.80515448811441));
#23305=CARTESIAN_POINT('Ctrl Pts',(5.30932343282159,63.5222500034686,-4.08005073111967));
#23306=CARTESIAN_POINT('Ctrl Pts',(4.05596218814318,63.3952500034686,-2.35494697412514));
#23307=CARTESIAN_POINT('Ctrl Pts',(2.02798109407154,63.2682500034685,-1.69601597307328));
#23308=CARTESIAN_POINT('Ctrl Pts',(0.,63.1412500034685,-1.0370849720215));
#23309=CARTESIAN_POINT('Ctrl Pts',(-2.02798109407154,63.0142500034686,-1.69601597307328));
#23310=CARTESIAN_POINT('Ctrl Pts',(-4.05596218814318,62.8872500034686,-2.35494697412514));
#23311=CARTESIAN_POINT('Ctrl Pts',(-5.30932343282164,62.7602500034687,-4.08005073111967));
#23312=CARTESIAN_POINT('Ctrl Pts',(-6.56268467749997,62.6332500034685,-5.80515448811441));
#23313=CARTESIAN_POINT('Ctrl Pts',(-6.56268467749999,62.5062500034685,-7.93749999999999));
#23314=CARTESIAN_POINT('Ctrl Pts',(-6.56268467750003,62.3792500034687,-10.0698455118856));
#23315=CARTESIAN_POINT('Ctrl Pts',(-5.30932343282159,62.2522500034686,-11.7949492688802));
#23316=CARTESIAN_POINT('Ctrl Pts',(-4.05596218814318,62.1252500034685,-13.5200530258749));
#23317=CARTESIAN_POINT('Ctrl Pts',(-2.02798109407148,61.9982500034687,-14.1789840269267));
#23318=CARTESIAN_POINT('Ctrl Pts',(0.,61.8712500034686,-14.8379150279786));
#23319=CARTESIAN_POINT('Ctrl Pts',(2.0279810940716,61.7442500034687,-14.1789840269267));
#23320=CARTESIAN_POINT('Ctrl Pts',(4.05596218814312,61.6172500034686,-13.5200530258749));
#23321=CARTESIAN_POINT('Ctrl Pts',(5.30932343282159,61.4902500034686,-11.7949492688802));
#23322=CARTESIAN_POINT('Ctrl Pts',(6.56268467749991,61.3632500034686,-10.0698455118856));
#23323=CARTESIAN_POINT('Ctrl Pts',(6.56268467749993,61.2362500034686,-7.93749999999999));
#23324=CARTESIAN_POINT('Origin',(-2.53888687851145E-9,74.888750003468,-7.9374999999999));
#23325=CARTESIAN_POINT('',(6.5626846775001,58.0612500034686,-7.93750000002823));
#23326=CARTESIAN_POINT('',(6.56268467749999,58.6962500034686,-7.93750000002716));
#23327=CARTESIAN_POINT('',(6.56268467242224,74.8887500034674,-7.93749999999981));
#23328=CARTESIAN_POINT('Ctrl Pts',(6.5626846775001,60.6012500034686,-7.93749999999999));
#23329=CARTESIAN_POINT('Ctrl Pts',(6.56268467750008,60.4742500034686,-5.80515448811441));
#23330=CARTESIAN_POINT('Ctrl Pts',(5.30932343282159,60.3472500034687,-4.08005073111967));
#23331=CARTESIAN_POINT('Ctrl Pts',(4.05596218814312,60.2202500034686,-2.35494697412514));
#23332=CARTESIAN_POINT('Ctrl Pts',(2.02798109407165,60.0932500034686,-1.69601597307328));
#23333=CARTESIAN_POINT('Ctrl Pts',(0.,59.9662500034686,-1.0370849720215));
#23334=CARTESIAN_POINT('Ctrl Pts',(-2.02798109407165,59.8392500034686,-1.69601597307317));
#23335=CARTESIAN_POINT('Ctrl Pts',(-4.05596218814306,59.7122500034685,-2.35494697412514));
#23336=CARTESIAN_POINT('Ctrl Pts',(-5.30932343282148,59.5852500034686,-4.08005073111967));
#23337=CARTESIAN_POINT('Ctrl Pts',(-6.56268467750003,59.4582500034686,-5.80515448811441));
#23338=CARTESIAN_POINT('Ctrl Pts',(-6.56268467750004,59.3312500034686,-7.93749999999999));
#23339=CARTESIAN_POINT('Ctrl Pts',(-6.56268467749991,59.2042500034686,-10.0698455118856));
#23340=CARTESIAN_POINT('Ctrl Pts',(-5.30932343282148,59.0772500034686,-11.7949492688802));
#23341=CARTESIAN_POINT('Ctrl Pts',(-4.05596218814312,58.9502500034686,-13.5200530258749));
#23342=CARTESIAN_POINT('Ctrl Pts',(-2.0279810940716,58.8232500034687,-14.1789840269267));
#23343=CARTESIAN_POINT('Ctrl Pts',(0.,58.6962500034686,-14.8379150279786));
#23344=CARTESIAN_POINT('Ctrl Pts',(2.0279810940716,58.5692500034687,-14.1789840269267));
#23345=CARTESIAN_POINT('Ctrl Pts',(4.05596218814318,58.4422500034685,-13.5200530258749));
#23346=CARTESIAN_POINT('Ctrl Pts',(5.30932343282159,58.3152500034686,-11.7949492688802));
#23347=CARTESIAN_POINT('Ctrl Pts',(6.56268467750003,58.1882500034686,-10.0698455118856));
#23348=CARTESIAN_POINT('Ctrl Pts',(6.5626846775001,58.0612500034686,-7.93749999999999));
#23349=CARTESIAN_POINT('Ctrl Pts',(6.56268467749993,61.2362500034686,-7.93749999999999));
#23350=CARTESIAN_POINT('Ctrl Pts',(6.56268467750003,61.1092500034686,-5.80515448811441));
#23351=CARTESIAN_POINT('Ctrl Pts',(5.30932343282159,60.9822500034687,-4.08005073111967));
#23352=CARTESIAN_POINT('Ctrl Pts',(4.05596218814306,60.8552500034686,-2.35494697412514));
#23353=CARTESIAN_POINT('Ctrl Pts',(2.02798109407154,60.7282500034685,-1.69601597307328));
#23354=CARTESIAN_POINT('Ctrl Pts',(0.,60.6012500034686,-1.0370849720215));
#23355=CARTESIAN_POINT('Ctrl Pts',(-2.02798109407154,60.4742500034686,-1.69601597307317));
#23356=CARTESIAN_POINT('Ctrl Pts',(-4.05596218814312,60.3472500034685,-2.35494697412514));
#23357=CARTESIAN_POINT('Ctrl Pts',(-5.30932343282159,60.2202500034686,-4.08005073111967));
#23358=CARTESIAN_POINT('Ctrl Pts',(-6.56268467749997,60.0932500034686,-5.80515448811441));
#23359=CARTESIAN_POINT('Ctrl Pts',(-6.56268467749999,59.9662500034687,-7.93749999999999));
#23360=CARTESIAN_POINT('Ctrl Pts',(-6.56268467750003,59.8392500034686,-10.0698455118856));
#23361=CARTESIAN_POINT('Ctrl Pts',(-5.30932343282159,59.7122500034685,-11.7949492688802));
#23362=CARTESIAN_POINT('Ctrl Pts',(-4.05596218814306,59.5852500034686,-13.5200530258749));
#23363=CARTESIAN_POINT('Ctrl Pts',(-2.02798109407148,59.4582500034687,-14.1789840269267));
#23364=CARTESIAN_POINT('Ctrl Pts',(1.1673575708729E-13,59.3312500034686,
-14.8379150279786));
#23365=CARTESIAN_POINT('Ctrl Pts',(2.02798109407148,59.2042500034687,-14.1789840269267));
#23366=CARTESIAN_POINT('Ctrl Pts',(4.05596218814324,59.0772500034685,-13.5200530258749));
#23367=CARTESIAN_POINT('Ctrl Pts',(5.30932343282159,58.9502500034686,-11.7949492688802));
#23368=CARTESIAN_POINT('Ctrl Pts',(6.56268467750008,58.8232500034686,-10.0698455118856));
#23369=CARTESIAN_POINT('Ctrl Pts',(6.56268467749999,58.6962500034686,-7.93749999999999));
#23370=CARTESIAN_POINT('Origin',(-2.53888687851145E-9,74.888750003468,-7.9374999999999));
#23371=CARTESIAN_POINT('',(6.5626846775001,55.5212500034686,-7.9375000000325));
#23372=CARTESIAN_POINT('',(6.56268467749999,56.1562500034686,-7.93750000003143));
#23373=CARTESIAN_POINT('',(6.56268467242224,74.8887500034674,-7.93749999999981));
#23374=CARTESIAN_POINT('Ctrl Pts',(6.5626846775001,58.0612500034686,-7.93749999999999));
#23375=CARTESIAN_POINT('Ctrl Pts',(6.56268467749997,57.9342500034686,-5.80515448811441));
#23376=CARTESIAN_POINT('Ctrl Pts',(5.30932343282164,57.8072500034686,-4.08005073111967));
#23377=CARTESIAN_POINT('Ctrl Pts',(4.05596218814318,57.6802500034686,-2.35494697412514));
#23378=CARTESIAN_POINT('Ctrl Pts',(2.02798109407154,57.5532500034686,-1.69601597307317));
#23379=CARTESIAN_POINT('Ctrl Pts',(0.,57.4262500034686,-1.0370849720215));
#23380=CARTESIAN_POINT('Ctrl Pts',(-2.0279810940716,57.2992500034686,-1.69601597307317));
#23381=CARTESIAN_POINT('Ctrl Pts',(-4.05596218814318,57.1722500034686,-2.35494697412514));
#23382=CARTESIAN_POINT('Ctrl Pts',(-5.30932343282148,57.0452500034685,-4.08005073111967));
#23383=CARTESIAN_POINT('Ctrl Pts',(-6.56268467749997,56.9182500034686,-5.80515448811441));
#23384=CARTESIAN_POINT('Ctrl Pts',(-6.56268467750004,56.7912500034686,-7.93749999999999));
#23385=CARTESIAN_POINT('Ctrl Pts',(-6.56268467750003,56.6642500034685,-10.0698455118856));
#23386=CARTESIAN_POINT('Ctrl Pts',(-5.30932343282159,56.5372500034686,-11.7949492688802));
#23387=CARTESIAN_POINT('Ctrl Pts',(-4.05596218814312,56.4102500034685,-13.5200530258749));
#23388=CARTESIAN_POINT('Ctrl Pts',(-2.0279810940716,56.2832500034686,-14.1789840269267));
#23389=CARTESIAN_POINT('Ctrl Pts',(0.,56.1562500034686,-14.8379150279786));
#23390=CARTESIAN_POINT('Ctrl Pts',(2.02798109407165,56.0292500034687,-14.1789840269267));
#23391=CARTESIAN_POINT('Ctrl Pts',(4.05596218814318,55.9022500034686,-13.5200530258749));
#23392=CARTESIAN_POINT('Ctrl Pts',(5.30932343282148,55.7752500034686,-11.7949492688802));
#23393=CARTESIAN_POINT('Ctrl Pts',(6.56268467750003,55.6482500034686,-10.0698455118856));
#23394=CARTESIAN_POINT('Ctrl Pts',(6.5626846775001,55.5212500034686,-7.93749999999999));
#23395=CARTESIAN_POINT('Ctrl Pts',(6.56268467749999,58.6962500034686,-7.93749999999999));
#23396=CARTESIAN_POINT('Ctrl Pts',(6.56268467750003,58.5692500034686,-5.80515448811441));
#23397=CARTESIAN_POINT('Ctrl Pts',(5.30932343282159,58.4422500034686,-4.08005073111967));
#23398=CARTESIAN_POINT('Ctrl Pts',(4.05596218814312,58.3152500034686,-2.35494697412514));
#23399=CARTESIAN_POINT('Ctrl Pts',(2.02798109407154,58.1882500034687,-1.69601597307328));
#23400=CARTESIAN_POINT('Ctrl Pts',(5.83678785436452E-14,58.0612500034686,
-1.0370849720215));
#23401=CARTESIAN_POINT('Ctrl Pts',(-2.02798109407154,57.9342500034686,-1.69601597307317));
#23402=CARTESIAN_POINT('Ctrl Pts',(-4.05596218814312,57.8072500034686,-2.35494697412514));
#23403=CARTESIAN_POINT('Ctrl Pts',(-5.30932343282159,57.6802500034686,-4.08005073111967));
#23404=CARTESIAN_POINT('Ctrl Pts',(-6.56268467750003,57.5532500034687,-5.80515448811441));
#23405=CARTESIAN_POINT('Ctrl Pts',(-6.56268467749993,57.4262500034687,-7.93749999999999));
#23406=CARTESIAN_POINT('Ctrl Pts',(-6.56268467749997,57.2992500034685,-10.0698455118856));
#23407=CARTESIAN_POINT('Ctrl Pts',(-5.30932343282159,57.1722500034686,-11.7949492688802));
#23408=CARTESIAN_POINT('Ctrl Pts',(-4.05596218814312,57.0452500034685,-13.5200530258749));
#23409=CARTESIAN_POINT('Ctrl Pts',(-2.0279810940716,56.9182500034687,-14.1789840269267));
#23410=CARTESIAN_POINT('Ctrl Pts',(0.,56.7912500034686,-14.8379150279786));
#23411=CARTESIAN_POINT('Ctrl Pts',(2.02798109407154,56.6642500034688,-14.1789840269267));
#23412=CARTESIAN_POINT('Ctrl Pts',(4.05596218814312,56.5372500034686,-13.5200530258749));
#23413=CARTESIAN_POINT('Ctrl Pts',(5.30932343282159,56.4102500034686,-11.7949492688802));
#23414=CARTESIAN_POINT('Ctrl Pts',(6.56268467750008,56.2832500034686,-10.0698455118856));
#23415=CARTESIAN_POINT('Ctrl Pts',(6.56268467749999,56.1562500034686,-7.93749999999999));
#23416=CARTESIAN_POINT('Origin',(-2.53888687851145E-9,74.888750003468,-7.9374999999999));
#23417=CARTESIAN_POINT('',(6.56268467749999,52.9812500034686,-7.93750000003681));
#23418=CARTESIAN_POINT('',(6.56268467749999,53.6162500034686,-7.93750000003573));
#23419=CARTESIAN_POINT('',(6.56268467242224,74.8887500034674,-7.93749999999981));
#23420=CARTESIAN_POINT('Ctrl Pts',(6.5626846775001,55.5212500034686,-7.93749999999999));
#23421=CARTESIAN_POINT('Ctrl Pts',(6.56268467750008,55.3942500034686,-5.80515448811441));
#23422=CARTESIAN_POINT('Ctrl Pts',(5.30932343282153,55.2672500034686,-4.08005073111967));
#23423=CARTESIAN_POINT('Ctrl Pts',(4.05596218814318,55.1402500034685,-2.35494697412514));
#23424=CARTESIAN_POINT('Ctrl Pts',(2.0279810940716,55.0132500034686,-1.69601597307317));
#23425=CARTESIAN_POINT('Ctrl Pts',(-5.83678785436452E-14,54.8862500034686,
-1.0370849720215));
#23426=CARTESIAN_POINT('Ctrl Pts',(-2.0279810940716,54.7592500034686,-1.69601597307323));
#23427=CARTESIAN_POINT('Ctrl Pts',(-4.05596218814318,54.6322500034686,-2.35494697412514));
#23428=CARTESIAN_POINT('Ctrl Pts',(-5.30932343282159,54.5052500034687,-4.08005073111972));
#23429=CARTESIAN_POINT('Ctrl Pts',(-6.56268467749997,54.3782500034686,-5.80515448811441));
#23430=CARTESIAN_POINT('Ctrl Pts',(-6.56268467749999,54.2512500034685,-7.93750000000004));
#23431=CARTESIAN_POINT('Ctrl Pts',(-6.56268467750003,54.1242500034686,-10.0698455118856));
#23432=CARTESIAN_POINT('Ctrl Pts',(-5.30932343282153,53.9972500034686,-11.7949492688803));
#23433=CARTESIAN_POINT('Ctrl Pts',(-4.05596218814318,53.8702500034686,-13.5200530258749));
#23434=CARTESIAN_POINT('Ctrl Pts',(-2.02798109407154,53.7432500034686,-14.1789840269267));
#23435=CARTESIAN_POINT('Ctrl Pts',(0.,53.6162500034685,-14.8379150279786));
#23436=CARTESIAN_POINT('Ctrl Pts',(2.02798109407165,53.4892500034686,-14.1789840269267));
#23437=CARTESIAN_POINT('Ctrl Pts',(4.05596218814312,53.3622500034686,-13.5200530258749));
#23438=CARTESIAN_POINT('Ctrl Pts',(5.30932343282153,53.2352500034686,-11.7949492688803));
#23439=CARTESIAN_POINT('Ctrl Pts',(6.56268467750003,53.1082500034686,-10.0698455118856));
#23440=CARTESIAN_POINT('Ctrl Pts',(6.56268467749999,52.9812500034686,-7.93750000000004));
#23441=CARTESIAN_POINT('Ctrl Pts',(6.56268467749999,56.1562500034686,-7.93749999999999));
#23442=CARTESIAN_POINT('Ctrl Pts',(6.56268467750003,56.0292500034686,-5.80515448811441));
#23443=CARTESIAN_POINT('Ctrl Pts',(5.30932343282164,55.9022500034686,-4.08005073111967));
#23444=CARTESIAN_POINT('Ctrl Pts',(4.05596218814324,55.7752500034686,-2.35494697412514));
#23445=CARTESIAN_POINT('Ctrl Pts',(2.0279810940716,55.6482500034686,-1.69601597307317));
#23446=CARTESIAN_POINT('Ctrl Pts',(0.,55.5212500034686,-1.0370849720215));
#23447=CARTESIAN_POINT('Ctrl Pts',(-2.02798109407148,55.3942500034686,-1.69601597307317));
#23448=CARTESIAN_POINT('Ctrl Pts',(-4.05596218814312,55.2672500034686,-2.35494697412514));
#23449=CARTESIAN_POINT('Ctrl Pts',(-5.30932343282159,55.1402500034686,-4.08005073111967));
#23450=CARTESIAN_POINT('Ctrl Pts',(-6.56268467749991,55.0132500034686,-5.80515448811441));
#23451=CARTESIAN_POINT('Ctrl Pts',(-6.56268467749987,54.8862500034686,-7.93750000000004));
#23452=CARTESIAN_POINT('Ctrl Pts',(-6.56268467749997,54.7592500034686,-10.0698455118856));
#23453=CARTESIAN_POINT('Ctrl Pts',(-5.30932343282153,54.6322500034687,-11.7949492688803));
#23454=CARTESIAN_POINT('Ctrl Pts',(-4.05596218814312,54.5052500034686,-13.5200530258749));
#23455=CARTESIAN_POINT('Ctrl Pts',(-2.02798109407154,54.3782500034687,-14.1789840269267));
#23456=CARTESIAN_POINT('Ctrl Pts',(0.,54.2512500034685,-14.8379150279786));
#23457=CARTESIAN_POINT('Ctrl Pts',(2.02798109407154,54.1242500034687,-14.1789840269267));
#23458=CARTESIAN_POINT('Ctrl Pts',(4.05596218814312,53.9972500034686,-13.5200530258749));
#23459=CARTESIAN_POINT('Ctrl Pts',(5.30932343282164,53.8702500034687,-11.7949492688803));
#23460=CARTESIAN_POINT('Ctrl Pts',(6.56268467749997,53.7432500034685,-10.0698455118856));
#23461=CARTESIAN_POINT('Ctrl Pts',(6.56268467749999,53.6162500034686,-7.93750000000004));
#23462=CARTESIAN_POINT('Origin',(-2.53888687851145E-9,74.888750003468,-7.9374999999999));
#23463=CARTESIAN_POINT('',(6.56268467749999,50.4412500034686,-7.93750000004108));
#23464=CARTESIAN_POINT('',(6.56268467749999,51.0762500034687,-7.93750000004001));
#23465=CARTESIAN_POINT('',(6.56268467242224,74.8887500034674,-7.93749999999981));
#23466=CARTESIAN_POINT('Ctrl Pts',(6.56268467749999,52.9812500034686,-7.93750000000004));
#23467=CARTESIAN_POINT('Ctrl Pts',(6.56268467749997,52.8542500034685,-5.80515448811441));
#23468=CARTESIAN_POINT('Ctrl Pts',(5.30932343282159,52.7272500034686,-4.08005073111972));
#23469=CARTESIAN_POINT('Ctrl Pts',(4.05596218814318,52.6002500034685,-2.35494697412514));
#23470=CARTESIAN_POINT('Ctrl Pts',(2.0279810940716,52.4732500034685,-1.69601597307323));
#23471=CARTESIAN_POINT('Ctrl Pts',(0.,52.3462500034685,-1.0370849720215));
#23472=CARTESIAN_POINT('Ctrl Pts',(-2.0279810940716,52.2192500034686,-1.69601597307323));
#23473=CARTESIAN_POINT('Ctrl Pts',(-4.05596218814318,52.0922500034686,-2.35494697412514));
#23474=CARTESIAN_POINT('Ctrl Pts',(-5.30932343282153,51.9652500034687,-4.08005073111972));
#23475=CARTESIAN_POINT('Ctrl Pts',(-6.56268467749997,51.8382500034685,-5.80515448811441));
#23476=CARTESIAN_POINT('Ctrl Pts',(-6.56268467749999,51.7112500034686,-7.93750000000004));
#23477=CARTESIAN_POINT('Ctrl Pts',(-6.56268467750003,51.5842500034685,-10.0698455118856));
#23478=CARTESIAN_POINT('Ctrl Pts',(-5.30932343282153,51.4572500034685,-11.7949492688803));
#23479=CARTESIAN_POINT('Ctrl Pts',(-4.05596218814306,51.3302500034686,-13.5200530258749));
#23480=CARTESIAN_POINT('Ctrl Pts',(-2.02798109407154,51.2032500034688,-14.1789840269267));
#23481=CARTESIAN_POINT('Ctrl Pts',(1.1673575708729E-13,51.0762500034686,
-14.8379150279786));
#23482=CARTESIAN_POINT('Ctrl Pts',(2.02798109407154,50.9492500034687,-14.1789840269267));
#23483=CARTESIAN_POINT('Ctrl Pts',(4.05596218814324,50.8222500034686,-13.5200530258749));
#23484=CARTESIAN_POINT('Ctrl Pts',(5.30932343282153,50.6952500034686,-11.7949492688803));
#23485=CARTESIAN_POINT('Ctrl Pts',(6.56268467750003,50.5682500034686,-10.0698455118856));
#23486=CARTESIAN_POINT('Ctrl Pts',(6.56268467749999,50.4412500034686,-7.93750000000004));
#23487=CARTESIAN_POINT('Ctrl Pts',(6.56268467749999,53.6162500034686,-7.93750000000004));
#23488=CARTESIAN_POINT('Ctrl Pts',(6.56268467750003,53.4892500034685,-5.80515448811441));
#23489=CARTESIAN_POINT('Ctrl Pts',(5.30932343282159,53.3622500034686,-4.08005073111972));
#23490=CARTESIAN_POINT('Ctrl Pts',(4.05596218814312,53.2352500034685,-2.35494697412514));
#23491=CARTESIAN_POINT('Ctrl Pts',(2.0279810940716,53.1082500034686,-1.69601597307323));
#23492=CARTESIAN_POINT('Ctrl Pts',(0.,52.9812500034685,-1.0370849720215));
#23493=CARTESIAN_POINT('Ctrl Pts',(-2.02798109407148,52.8542500034686,-1.69601597307323));
#23494=CARTESIAN_POINT('Ctrl Pts',(-4.05596218814312,52.7272500034686,-2.35494697412514));
#23495=CARTESIAN_POINT('Ctrl Pts',(-5.30932343282159,52.6002500034685,-4.08005073111972));
#23496=CARTESIAN_POINT('Ctrl Pts',(-6.56268467750003,52.4732500034686,-5.80515448811441));
#23497=CARTESIAN_POINT('Ctrl Pts',(-6.56268467749999,52.3462500034686,-7.93750000000004));
#23498=CARTESIAN_POINT('Ctrl Pts',(-6.56268467749997,52.2192500034685,-10.0698455118856));
#23499=CARTESIAN_POINT('Ctrl Pts',(-5.30932343282153,52.0922500034686,-11.7949492688803));
#23500=CARTESIAN_POINT('Ctrl Pts',(-4.05596218814312,51.9652500034685,-13.5200530258749));
#23501=CARTESIAN_POINT('Ctrl Pts',(-2.02798109407154,51.8382500034687,-14.1789840269267));
#23502=CARTESIAN_POINT('Ctrl Pts',(0.,51.7112500034685,-14.8379150279786));
#23503=CARTESIAN_POINT('Ctrl Pts',(2.02798109407154,51.5842500034687,-14.1789840269267));
#23504=CARTESIAN_POINT('Ctrl Pts',(4.05596218814312,51.4572500034685,-13.5200530258749));
#23505=CARTESIAN_POINT('Ctrl Pts',(5.30932343282164,51.3302500034686,-11.7949492688803));
#23506=CARTESIAN_POINT('Ctrl Pts',(6.56268467750008,51.2032500034686,-10.0698455118856));
#23507=CARTESIAN_POINT('Ctrl Pts',(6.56268467749999,51.0762500034687,-7.93750000000004));
#23508=CARTESIAN_POINT('Origin',(-2.53888687851145E-9,74.888750003468,-7.9374999999999));
#23509=CARTESIAN_POINT('',(6.56268467750004,47.9012500034686,-7.93750000004536));
#23510=CARTESIAN_POINT('',(6.56268467750004,48.5362500034686,-7.93750000004429));
#23511=CARTESIAN_POINT('',(6.56268467242224,74.8887500034674,-7.93749999999981));
#23512=CARTESIAN_POINT('Ctrl Pts',(6.56268467749999,50.4412500034686,-7.93750000000004));
#23513=CARTESIAN_POINT('Ctrl Pts',(6.56268467750003,50.3142500034686,-5.80515448811441));
#23514=CARTESIAN_POINT('Ctrl Pts',(5.30932343282159,50.1872500034685,-4.08005073111972));
#23515=CARTESIAN_POINT('Ctrl Pts',(4.05596218814318,50.0602500034686,-2.35494697412514));
#23516=CARTESIAN_POINT('Ctrl Pts',(2.0279810940716,49.9332500034686,-1.69601597307323));
#23517=CARTESIAN_POINT('Ctrl Pts',(1.1673575708729E-13,49.8062500034686,
-1.0370849720215));
#23518=CARTESIAN_POINT('Ctrl Pts',(-2.0279810940716,49.6792500034686,-1.69601597307323));
#23519=CARTESIAN_POINT('Ctrl Pts',(-4.05596218814312,49.5522500034686,-2.35494697412514));
#23520=CARTESIAN_POINT('Ctrl Pts',(-5.30932343282153,49.4252500034686,-4.08005073111972));
#23521=CARTESIAN_POINT('Ctrl Pts',(-6.56268467750008,49.2982500034686,-5.80515448811441));
#23522=CARTESIAN_POINT('Ctrl Pts',(-6.56268467749999,49.1712500034686,-7.93750000000004));
#23523=CARTESIAN_POINT('Ctrl Pts',(-6.56268467750003,49.0442500034686,-10.0698455118856));
#23524=CARTESIAN_POINT('Ctrl Pts',(-5.30932343282148,48.9172500034685,-11.7949492688803));
#23525=CARTESIAN_POINT('Ctrl Pts',(-4.05596218814318,48.7902500034686,-13.5200530258749));
#23526=CARTESIAN_POINT('Ctrl Pts',(-2.02798109407165,48.6632500034687,-14.1789840269267));
#23527=CARTESIAN_POINT('Ctrl Pts',(0.,48.5362500034685,-14.8379150279786));
#23528=CARTESIAN_POINT('Ctrl Pts',(2.0279810940716,48.4092500034688,-14.1789840269267));
#23529=CARTESIAN_POINT('Ctrl Pts',(4.05596218814312,48.2822500034686,-13.5200530258749));
#23530=CARTESIAN_POINT('Ctrl Pts',(5.30932343282159,48.1552500034686,-11.7949492688803));
#23531=CARTESIAN_POINT('Ctrl Pts',(6.56268467750008,48.0282500034685,-10.0698455118856));
#23532=CARTESIAN_POINT('Ctrl Pts',(6.56268467750004,47.9012500034686,-7.93750000000004));
#23533=CARTESIAN_POINT('Ctrl Pts',(6.56268467749999,51.0762500034687,-7.93750000000004));
#23534=CARTESIAN_POINT('Ctrl Pts',(6.56268467749997,50.9492500034685,-5.80515448811441));
#23535=CARTESIAN_POINT('Ctrl Pts',(5.30932343282159,50.8222500034686,-4.08005073111972));
#23536=CARTESIAN_POINT('Ctrl Pts',(4.05596218814312,50.6952500034686,-2.35494697412514));
#23537=CARTESIAN_POINT('Ctrl Pts',(2.0279810940716,50.5682500034686,-1.69601597307323));
#23538=CARTESIAN_POINT('Ctrl Pts',(0.,50.4412500034686,-1.0370849720215));
#23539=CARTESIAN_POINT('Ctrl Pts',(-2.0279810940716,50.3142500034687,-1.69601597307323));
#23540=CARTESIAN_POINT('Ctrl Pts',(-4.05596218814312,50.1872500034686,-2.35494697412514));
#23541=CARTESIAN_POINT('Ctrl Pts',(-5.30932343282153,50.0602500034686,-4.08005073111972));
#23542=CARTESIAN_POINT('Ctrl Pts',(-6.56268467750003,49.9332500034686,-5.80515448811441));
#23543=CARTESIAN_POINT('Ctrl Pts',(-6.56268467749999,49.8062500034686,-7.93750000000004));
#23544=CARTESIAN_POINT('Ctrl Pts',(-6.56268467749997,49.6792500034685,-10.0698455118856));
#23545=CARTESIAN_POINT('Ctrl Pts',(-5.30932343282159,49.5522500034686,-11.7949492688803));
#23546=CARTESIAN_POINT('Ctrl Pts',(-4.05596218814312,49.4252500034686,-13.5200530258749));
#23547=CARTESIAN_POINT('Ctrl Pts',(-2.02798109407154,49.2982500034686,-14.1789840269267));
#23548=CARTESIAN_POINT('Ctrl Pts',(0.,49.1712500034685,-14.8379150279786));
#23549=CARTESIAN_POINT('Ctrl Pts',(2.0279810940716,49.0442500034687,-14.1789840269267));
#23550=CARTESIAN_POINT('Ctrl Pts',(4.05596218814318,48.9172500034685,-13.5200530258749));
#23551=CARTESIAN_POINT('Ctrl Pts',(5.30932343282159,48.7902500034686,-11.7949492688803));
#23552=CARTESIAN_POINT('Ctrl Pts',(6.56268467750003,48.6632500034685,-10.0698455118856));
#23553=CARTESIAN_POINT('Ctrl Pts',(6.56268467750004,48.5362500034686,-7.93750000000004));
#23554=CARTESIAN_POINT('Origin',(-2.53888687851145E-9,74.888750003468,-7.9374999999999));
#23555=CARTESIAN_POINT('',(6.5626846775001,45.3612500034686,-7.93750000004963));
#23556=CARTESIAN_POINT('',(6.56268467749993,45.9962500034686,-7.93750000004856));
#23557=CARTESIAN_POINT('',(6.56268467242224,74.8887500034674,-7.93749999999981));
#23558=CARTESIAN_POINT('Ctrl Pts',(6.56268467750004,47.9012500034686,-7.93750000000004));
#23559=CARTESIAN_POINT('Ctrl Pts',(6.56268467750003,47.7742500034685,-5.80515448811441));
#23560=CARTESIAN_POINT('Ctrl Pts',(5.30932343282159,47.6472500034686,-4.08005073111972));
#23561=CARTESIAN_POINT('Ctrl Pts',(4.05596218814324,47.5202500034686,-2.35494697412514));
#23562=CARTESIAN_POINT('Ctrl Pts',(2.02798109407165,47.3932500034687,-1.69601597307323));
#23563=CARTESIAN_POINT('Ctrl Pts',(0.,47.2662500034685,-1.0370849720215));
#23564=CARTESIAN_POINT('Ctrl Pts',(-2.02798109407154,47.1392500034686,-1.69601597307323));
#23565=CARTESIAN_POINT('Ctrl Pts',(-4.05596218814312,47.0122500034686,-2.35494697412514));
#23566=CARTESIAN_POINT('Ctrl Pts',(-5.30932343282148,46.8852500034686,-4.08005073111972));
#23567=CARTESIAN_POINT('Ctrl Pts',(-6.56268467749991,46.7582500034685,-5.80515448811441));
#23568=CARTESIAN_POINT('Ctrl Pts',(-6.56268467749999,46.6312500034686,-7.93750000000004));
#23569=CARTESIAN_POINT('Ctrl Pts',(-6.56268467749997,46.5042500034685,-10.0698455118856));
#23570=CARTESIAN_POINT('Ctrl Pts',(-5.30932343282148,46.3772500034686,-11.7949492688803));
#23571=CARTESIAN_POINT('Ctrl Pts',(-4.05596218814312,46.2502500034686,-13.5200530258749));
#23572=CARTESIAN_POINT('Ctrl Pts',(-2.0279810940716,46.1232500034687,-14.1789840269267));
#23573=CARTESIAN_POINT('Ctrl Pts',(0.,45.9962500034684,-14.8379150279786));
#23574=CARTESIAN_POINT('Ctrl Pts',(2.0279810940716,45.8692500034687,-14.1789840269267));
#23575=CARTESIAN_POINT('Ctrl Pts',(4.05596218814312,45.7422500034686,-13.5200530258749));
#23576=CARTESIAN_POINT('Ctrl Pts',(5.30932343282159,45.6152500034686,-11.7949492688803));
#23577=CARTESIAN_POINT('Ctrl Pts',(6.56268467749997,45.4882500034686,-10.0698455118856));
#23578=CARTESIAN_POINT('Ctrl Pts',(6.5626846775001,45.3612500034686,-7.93750000000004));
#23579=CARTESIAN_POINT('Ctrl Pts',(6.56268467750004,48.5362500034686,-7.93750000000004));
#23580=CARTESIAN_POINT('Ctrl Pts',(6.56268467750008,48.4092500034685,-5.80515448811441));
#23581=CARTESIAN_POINT('Ctrl Pts',(5.30932343282159,48.2822500034686,-4.08005073111972));
#23582=CARTESIAN_POINT('Ctrl Pts',(4.05596218814312,48.1552500034686,-2.35494697412514));
#23583=CARTESIAN_POINT('Ctrl Pts',(2.02798109407154,48.0282500034685,-1.69601597307323));
#23584=CARTESIAN_POINT('Ctrl Pts',(0.,47.9012500034685,-1.0370849720215));
#23585=CARTESIAN_POINT('Ctrl Pts',(-2.02798109407154,47.7742500034686,-1.69601597307323));
#23586=CARTESIAN_POINT('Ctrl Pts',(-4.05596218814318,47.6472500034685,-2.35494697412514));
#23587=CARTESIAN_POINT('Ctrl Pts',(-5.30932343282153,47.5202500034686,-4.08005073111972));
#23588=CARTESIAN_POINT('Ctrl Pts',(-6.56268467750003,47.3932500034686,-5.80515448811441));
#23589=CARTESIAN_POINT('Ctrl Pts',(-6.56268467749999,47.2662500034685,-7.93750000000004));
#23590=CARTESIAN_POINT('Ctrl Pts',(-6.56268467750003,47.1392500034685,-10.0698455118856));
#23591=CARTESIAN_POINT('Ctrl Pts',(-5.30932343282159,47.0122500034686,-11.7949492688803));
#23592=CARTESIAN_POINT('Ctrl Pts',(-4.05596218814324,46.8852500034686,-13.5200530258749));
#23593=CARTESIAN_POINT('Ctrl Pts',(-2.02798109407148,46.7582500034687,-14.1789840269267));
#23594=CARTESIAN_POINT('Ctrl Pts',(-1.1673575708729E-13,46.6312500034685,
-14.8379150279786));
#23595=CARTESIAN_POINT('Ctrl Pts',(2.0279810940716,46.5042500034687,-14.1789840269267));
#23596=CARTESIAN_POINT('Ctrl Pts',(4.05596218814318,46.3772500034686,-13.5200530258749));
#23597=CARTESIAN_POINT('Ctrl Pts',(5.30932343282159,46.2502500034686,-11.7949492688803));
#23598=CARTESIAN_POINT('Ctrl Pts',(6.56268467750003,46.1232500034686,-10.0698455118856));
#23599=CARTESIAN_POINT('Ctrl Pts',(6.56268467749993,45.9962500034686,-7.93750000000004));
#23600=CARTESIAN_POINT('Origin',(-2.53888687851145E-9,74.888750003468,-7.9374999999999));
#23601=CARTESIAN_POINT('',(6.5626846775001,42.8212500034686,-7.93750000005391));
#23602=CARTESIAN_POINT('',(6.56268467749999,43.4562500034686,-7.93750000005284));
#23603=CARTESIAN_POINT('',(6.56268467242224,74.8887500034674,-7.93749999999981));
#23604=CARTESIAN_POINT('Ctrl Pts',(6.5626846775001,45.3612500034686,-7.93750000000004));
#23605=CARTESIAN_POINT('Ctrl Pts',(6.56268467750003,45.2342500034686,-5.80515448811441));
#23606=CARTESIAN_POINT('Ctrl Pts',(5.30932343282153,45.1072500034687,-4.08005073111972));
#23607=CARTESIAN_POINT('Ctrl Pts',(4.05596218814312,44.9802500034686,-2.35494697412514));
#23608=CARTESIAN_POINT('Ctrl Pts',(2.02798109407165,44.8532500034686,-1.69601597307323));
#23609=CARTESIAN_POINT('Ctrl Pts',(0.,44.7262500034686,-1.0370849720215));
#23610=CARTESIAN_POINT('Ctrl Pts',(-2.02798109407154,44.5992500034686,-1.69601597307323));
#23611=CARTESIAN_POINT('Ctrl Pts',(-4.05596218814312,44.4722500034685,-2.35494697412514));
#23612=CARTESIAN_POINT('Ctrl Pts',(-5.30932343282148,44.3452500034686,-4.08005073111972));
#23613=CARTESIAN_POINT('Ctrl Pts',(-6.56268467750003,44.2182500034685,-5.80515448811441));
#23614=CARTESIAN_POINT('Ctrl Pts',(-6.56268467750004,44.0912500034686,-7.93750000000004));
#23615=CARTESIAN_POINT('Ctrl Pts',(-6.56268467749997,43.9642500034686,-10.0698455118856));
#23616=CARTESIAN_POINT('Ctrl Pts',(-5.30932343282148,43.8372500034686,-11.7949492688803));
#23617=CARTESIAN_POINT('Ctrl Pts',(-4.05596218814312,43.7102500034686,-13.5200530258749));
#23618=CARTESIAN_POINT('Ctrl Pts',(-2.0279810940716,43.5832500034687,-14.1789840269267));
#23619=CARTESIAN_POINT('Ctrl Pts',(0.,43.4562500034686,-14.8379150279786));
#23620=CARTESIAN_POINT('Ctrl Pts',(2.0279810940716,43.3292500034687,-14.1789840269267));
#23621=CARTESIAN_POINT('Ctrl Pts',(4.05596218814312,43.2022500034684,-13.5200530258749));
#23622=CARTESIAN_POINT('Ctrl Pts',(5.30932343282159,43.0752500034686,-11.7949492688803));
#23623=CARTESIAN_POINT('Ctrl Pts',(6.56268467750008,42.9482500034686,-10.0698455118856));
#23624=CARTESIAN_POINT('Ctrl Pts',(6.5626846775001,42.8212500034686,-7.93750000000004));
#23625=CARTESIAN_POINT('Ctrl Pts',(6.56268467749993,45.9962500034686,-7.93750000000004));
#23626=CARTESIAN_POINT('Ctrl Pts',(6.56268467750008,45.8692500034686,-5.80515448811441));
#23627=CARTESIAN_POINT('Ctrl Pts',(5.30932343282159,45.7422500034685,-4.08005073111972));
#23628=CARTESIAN_POINT('Ctrl Pts',(4.05596218814318,45.6152500034686,-2.35494697412514));
#23629=CARTESIAN_POINT('Ctrl Pts',(2.02798109407154,45.4882500034685,-1.69601597307323));
#23630=CARTESIAN_POINT('Ctrl Pts',(-1.1673575708729E-13,45.3612500034685,
-1.0370849720215));
#23631=CARTESIAN_POINT('Ctrl Pts',(-2.02798109407154,45.2342500034686,-1.69601597307323));
#23632=CARTESIAN_POINT('Ctrl Pts',(-4.05596218814306,45.1072500034685,-2.35494697412514));
#23633=CARTESIAN_POINT('Ctrl Pts',(-5.30932343282159,44.9802500034686,-4.08005073111972));
#23634=CARTESIAN_POINT('Ctrl Pts',(-6.56268467749997,44.8532500034685,-5.80515448811441));
#23635=CARTESIAN_POINT('Ctrl Pts',(-6.56268467749993,44.7262500034686,-7.93750000000004));
#23636=CARTESIAN_POINT('Ctrl Pts',(-6.56268467749991,44.5992500034686,-10.0698455118856));
#23637=CARTESIAN_POINT('Ctrl Pts',(-5.30932343282159,44.4722500034685,-11.7949492688803));
#23638=CARTESIAN_POINT('Ctrl Pts',(-4.05596218814306,44.3452500034686,-13.5200530258749));
#23639=CARTESIAN_POINT('Ctrl Pts',(-2.02798109407148,44.2182500034687,-14.1789840269267));
#23640=CARTESIAN_POINT('Ctrl Pts',(0.,44.0912500034687,-14.8379150279786));
#23641=CARTESIAN_POINT('Ctrl Pts',(2.0279810940716,43.9642500034687,-14.1789840269267));
#23642=CARTESIAN_POINT('Ctrl Pts',(4.05596218814318,43.8372500034685,-13.5200530258749));
#23643=CARTESIAN_POINT('Ctrl Pts',(5.30932343282159,43.7102500034686,-11.7949492688803));
#23644=CARTESIAN_POINT('Ctrl Pts',(6.56268467750003,43.5832500034686,-10.0698455118856));
#23645=CARTESIAN_POINT('Ctrl Pts',(6.56268467749999,43.4562500034686,-7.93750000000004));
#23646=CARTESIAN_POINT('Origin',(-2.53888687851145E-9,74.888750003468,-7.9374999999999));
#23647=CARTESIAN_POINT('',(6.5626846775001,40.2812500034686,-7.93750000005818));
#23648=CARTESIAN_POINT('',(6.56268467749999,40.9162500034685,-7.93750000005712));
#23649=CARTESIAN_POINT('',(6.56268467242224,74.8887500034674,-7.93749999999981));
#23650=CARTESIAN_POINT('Ctrl Pts',(6.5626846775001,42.8212500034686,-7.93750000000004));
#23651=CARTESIAN_POINT('Ctrl Pts',(6.56268467750003,42.6942500034686,-5.80515448811441));
#23652=CARTESIAN_POINT('Ctrl Pts',(5.30932343282153,42.5672500034686,-4.08005073111972));
#23653=CARTESIAN_POINT('Ctrl Pts',(4.05596218814324,42.4402500034686,-2.35494697412514));
#23654=CARTESIAN_POINT('Ctrl Pts',(2.02798109407165,42.3132500034686,-1.69601597307323));
#23655=CARTESIAN_POINT('Ctrl Pts',(0.,42.1862500034686,-1.0370849720215));
#23656=CARTESIAN_POINT('Ctrl Pts',(-2.0279810940716,42.0592500034685,-1.69601597307323));
#23657=CARTESIAN_POINT('Ctrl Pts',(-4.05596218814312,41.9322500034686,-2.35494697412514));
#23658=CARTESIAN_POINT('Ctrl Pts',(-5.30932343282148,41.8052500034685,-4.08005073111972));
#23659=CARTESIAN_POINT('Ctrl Pts',(-6.56268467750003,41.6782500034686,-5.80515448811441));
#23660=CARTESIAN_POINT('Ctrl Pts',(-6.56268467750004,41.5512500034686,-7.93750000000004));
#23661=CARTESIAN_POINT('Ctrl Pts',(-6.56268467749997,41.4242500034686,-10.0698455118856));
#23662=CARTESIAN_POINT('Ctrl Pts',(-5.30932343282153,41.2972500034686,-11.7949492688803));
#23663=CARTESIAN_POINT('Ctrl Pts',(-4.05596218814312,41.1702500034685,-13.5200530258749));
#23664=CARTESIAN_POINT('Ctrl Pts',(-2.0279810940716,41.0432500034686,-14.1789840269267));
#23665=CARTESIAN_POINT('Ctrl Pts',(0.,40.9162500034686,-14.8379150279786));
#23666=CARTESIAN_POINT('Ctrl Pts',(2.02798109407165,40.7892500034687,-14.1789840269267));
#23667=CARTESIAN_POINT('Ctrl Pts',(4.05596218814312,40.6622500034685,-13.5200530258749));
#23668=CARTESIAN_POINT('Ctrl Pts',(5.30932343282153,40.5352500034686,-11.7949492688803));
#23669=CARTESIAN_POINT('Ctrl Pts',(6.56268467749997,40.4082500034686,-10.0698455118856));
#23670=CARTESIAN_POINT('Ctrl Pts',(6.5626846775001,40.2812500034686,-7.93750000000004));
#23671=CARTESIAN_POINT('Ctrl Pts',(6.56268467749999,43.4562500034686,-7.93750000000004));
#23672=CARTESIAN_POINT('Ctrl Pts',(6.56268467749997,43.3292500034686,-5.80515448811441));
#23673=CARTESIAN_POINT('Ctrl Pts',(5.30932343282164,43.2022500034686,-4.08005073111972));
#23674=CARTESIAN_POINT('Ctrl Pts',(4.05596218814306,43.0752500034686,-2.35494697412514));
#23675=CARTESIAN_POINT('Ctrl Pts',(2.02798109407154,42.9482500034687,-1.69601597307323));
#23676=CARTESIAN_POINT('Ctrl Pts',(1.1673575708729E-13,42.8212500034686,
-1.0370849720215));
#23677=CARTESIAN_POINT('Ctrl Pts',(-2.02798109407154,42.6942500034686,-1.69601597307323));
#23678=CARTESIAN_POINT('Ctrl Pts',(-4.05596218814318,42.5672500034685,-2.35494697412514));
#23679=CARTESIAN_POINT('Ctrl Pts',(-5.30932343282159,42.4402500034686,-4.08005073111972));
#23680=CARTESIAN_POINT('Ctrl Pts',(-6.56268467749997,42.3132500034686,-5.80515448811441));
#23681=CARTESIAN_POINT('Ctrl Pts',(-6.56268467749993,42.1862500034687,-7.93750000000004));
#23682=CARTESIAN_POINT('Ctrl Pts',(-6.56268467750003,42.0592500034685,-10.0698455118856));
#23683=CARTESIAN_POINT('Ctrl Pts',(-5.30932343282159,41.9322500034685,-11.7949492688803));
#23684=CARTESIAN_POINT('Ctrl Pts',(-4.05596218814306,41.8052500034685,-13.5200530258749));
#23685=CARTESIAN_POINT('Ctrl Pts',(-2.02798109407148,41.6782500034687,-14.1789840269267));
#23686=CARTESIAN_POINT('Ctrl Pts',(1.1673575708729E-13,41.5512500034686,
-14.8379150279786));
#23687=CARTESIAN_POINT('Ctrl Pts',(2.02798109407154,41.4242500034688,-14.1789840269267));
#23688=CARTESIAN_POINT('Ctrl Pts',(4.05596218814324,41.2972500034684,-13.5200530258749));
#23689=CARTESIAN_POINT('Ctrl Pts',(5.30932343282159,41.1702500034686,-11.7949492688803));
#23690=CARTESIAN_POINT('Ctrl Pts',(6.56268467750003,41.0432500034686,-10.0698455118856));
#23691=CARTESIAN_POINT('Ctrl Pts',(6.56268467749999,40.9162500034685,-7.93750000000004));
#23692=CARTESIAN_POINT('Origin',(-2.53888687851145E-9,74.888750003468,-7.9374999999999));
#23693=CARTESIAN_POINT('',(6.56268467749999,37.7412500034686,-7.93750000006246));
#23694=CARTESIAN_POINT('',(6.56268467749999,38.3762500034686,-7.93750000006139));
#23695=CARTESIAN_POINT('',(6.56268467242224,74.8887500034674,-7.93749999999981));
#23696=CARTESIAN_POINT('Ctrl Pts',(6.5626846775001,40.2812500034686,-7.93750000000004));
#23697=CARTESIAN_POINT('Ctrl Pts',(6.56268467750008,40.1542500034685,-5.80515448811441));
#23698=CARTESIAN_POINT('Ctrl Pts',(5.30932343282153,40.0272500034686,-4.08005073111972));
#23699=CARTESIAN_POINT('Ctrl Pts',(4.05596218814312,39.9002500034686,-2.35494697412514));
#23700=CARTESIAN_POINT('Ctrl Pts',(2.0279810940716,39.7732500034685,-1.69601597307323));
#23701=CARTESIAN_POINT('Ctrl Pts',(0.,39.6462500034686,-1.0370849720215));
#23702=CARTESIAN_POINT('Ctrl Pts',(-2.0279810940716,39.5192500034686,-1.69601597307323));
#23703=CARTESIAN_POINT('Ctrl Pts',(-4.05596218814324,39.3922500034686,-2.35494697412514));
#23704=CARTESIAN_POINT('Ctrl Pts',(-5.30932343282148,39.2652500034686,-4.08005073111972));
#23705=CARTESIAN_POINT('Ctrl Pts',(-6.56268467749991,39.1382500034686,-5.80515448811441));
#23706=CARTESIAN_POINT('Ctrl Pts',(-6.56268467749999,39.0112500034685,-7.93750000000004));
#23707=CARTESIAN_POINT('Ctrl Pts',(-6.56268467750008,38.8842500034686,-10.0698455118856));
#23708=CARTESIAN_POINT('Ctrl Pts',(-5.30932343282153,38.7572500034686,-11.7949492688803));
#23709=CARTESIAN_POINT('Ctrl Pts',(-4.05596218814312,38.6302500034686,-13.5200530258749));
#23710=CARTESIAN_POINT('Ctrl Pts',(-2.02798109407154,38.5032500034686,-14.1789840269267));
#23711=CARTESIAN_POINT('Ctrl Pts',(0.,38.3762500034685,-14.8379150279786));
#23712=CARTESIAN_POINT('Ctrl Pts',(2.02798109407165,38.2492500034686,-14.1789840269267));
#23713=CARTESIAN_POINT('Ctrl Pts',(4.05596218814318,38.1222500034686,-13.5200530258749));
#23714=CARTESIAN_POINT('Ctrl Pts',(5.30932343282153,37.9952500034686,-11.7949492688803));
#23715=CARTESIAN_POINT('Ctrl Pts',(6.56268467750003,37.8682500034686,-10.0698455118856));
#23716=CARTESIAN_POINT('Ctrl Pts',(6.56268467749999,37.7412500034686,-7.93750000000004));
#23717=CARTESIAN_POINT('Ctrl Pts',(6.56268467749999,40.9162500034685,-7.93750000000004));
#23718=CARTESIAN_POINT('Ctrl Pts',(6.56268467750014,40.7892500034686,-5.80515448811441));
#23719=CARTESIAN_POINT('Ctrl Pts',(5.30932343282164,40.6622500034686,-4.08005073111972));
#23720=CARTESIAN_POINT('Ctrl Pts',(4.05596218814318,40.5352500034686,-2.35494697412514));
#23721=CARTESIAN_POINT('Ctrl Pts',(2.0279810940716,40.4082500034686,-1.69601597307323));
#23722=CARTESIAN_POINT('Ctrl Pts',(0.,40.2812500034686,-1.0370849720215));
#23723=CARTESIAN_POINT('Ctrl Pts',(-2.02798109407148,40.1542500034686,-1.69601597307323));
#23724=CARTESIAN_POINT('Ctrl Pts',(-4.05596218814312,40.0272500034685,-2.35494697412514));
#23725=CARTESIAN_POINT('Ctrl Pts',(-5.30932343282159,39.9002500034686,-4.08005073111972));
#23726=CARTESIAN_POINT('Ctrl Pts',(-6.56268467749997,39.7732500034686,-5.80515448811441));
#23727=CARTESIAN_POINT('Ctrl Pts',(-6.56268467749987,39.6462500034686,-7.93750000000004));
#23728=CARTESIAN_POINT('Ctrl Pts',(-6.56268467750003,39.5192500034686,-10.0698455118856));
#23729=CARTESIAN_POINT('Ctrl Pts',(-5.30932343282153,39.3922500034687,-11.7949492688803));
#23730=CARTESIAN_POINT('Ctrl Pts',(-4.05596218814318,39.2652500034686,-13.5200530258749));
#23731=CARTESIAN_POINT('Ctrl Pts',(-2.02798109407154,39.1382500034687,-14.1789840269267));
#23732=CARTESIAN_POINT('Ctrl Pts',(0.,39.0112500034685,-14.8379150279786));
#23733=CARTESIAN_POINT('Ctrl Pts',(2.02798109407154,38.8842500034687,-14.1789840269267));
#23734=CARTESIAN_POINT('Ctrl Pts',(4.05596218814312,38.7572500034686,-13.5200530258749));
#23735=CARTESIAN_POINT('Ctrl Pts',(5.30932343282164,38.6302500034687,-11.7949492688803));
#23736=CARTESIAN_POINT('Ctrl Pts',(6.56268467749991,38.5032500034686,-10.0698455118856));
#23737=CARTESIAN_POINT('Ctrl Pts',(6.56268467749999,38.3762500034686,-7.93750000000004));
#23738=CARTESIAN_POINT('Origin',(-2.53888687851145E-9,74.888750003468,-7.9374999999999));
#23739=CARTESIAN_POINT('',(6.56268467749999,35.2012500034686,-7.93750000006674));
#23740=CARTESIAN_POINT('',(6.56268467749999,35.8362500034687,-7.93750000006567));
#23741=CARTESIAN_POINT('',(6.56268467242224,74.8887500034674,-7.93749999999981));
#23742=CARTESIAN_POINT('Ctrl Pts',(6.56268467749999,37.7412500034686,-7.93750000000004));
#23743=CARTESIAN_POINT('Ctrl Pts',(6.56268467750008,37.6142500034686,-5.80515448811441));
#23744=CARTESIAN_POINT('Ctrl Pts',(5.30932343282159,37.4872500034686,-4.08005073111972));
#23745=CARTESIAN_POINT('Ctrl Pts',(4.05596218814312,37.3602500034685,-2.35494697412514));
#23746=CARTESIAN_POINT('Ctrl Pts',(2.0279810940716,37.2332500034685,-1.69601597307323));
#23747=CARTESIAN_POINT('Ctrl Pts',(-1.1673575708729E-13,37.1062500034685,
-1.0370849720215));
#23748=CARTESIAN_POINT('Ctrl Pts',(-2.0279810940716,36.9792500034686,-1.69601597307323));
#23749=CARTESIAN_POINT('Ctrl Pts',(-4.05596218814306,36.8522500034687,-2.35494697412514));
#23750=CARTESIAN_POINT('Ctrl Pts',(-5.30932343282153,36.7252500034687,-4.08005073111972));
#23751=CARTESIAN_POINT('Ctrl Pts',(-6.56268467750003,36.5982500034685,-5.80515448811441));
#23752=CARTESIAN_POINT('Ctrl Pts',(-6.56268467749999,36.4712500034686,-7.93750000000004));
#23753=CARTESIAN_POINT('Ctrl Pts',(-6.56268467749991,36.3442500034685,-10.0698455118856));
#23754=CARTESIAN_POINT('Ctrl Pts',(-5.30932343282153,36.2172500034686,-11.7949492688803));
#23755=CARTESIAN_POINT('Ctrl Pts',(-4.05596218814312,36.0902500034685,-13.5200530258749));
#23756=CARTESIAN_POINT('Ctrl Pts',(-2.02798109407154,35.9632500034688,-14.1789840269267));
#23757=CARTESIAN_POINT('Ctrl Pts',(0.,35.8362500034686,-14.8379150279786));
#23758=CARTESIAN_POINT('Ctrl Pts',(2.02798109407165,35.7092500034686,-14.1789840269267));
#23759=CARTESIAN_POINT('Ctrl Pts',(4.05596218814318,35.5822500034686,-13.5200530258749));
#23760=CARTESIAN_POINT('Ctrl Pts',(5.30932343282153,35.4552500034687,-11.7949492688803));
#23761=CARTESIAN_POINT('Ctrl Pts',(6.56268467750003,35.3282500034686,-10.0698455118856));
#23762=CARTESIAN_POINT('Ctrl Pts',(6.56268467749999,35.2012500034686,-7.93750000000004));
#23763=CARTESIAN_POINT('Ctrl Pts',(6.56268467749999,38.3762500034686,-7.93750000000004));
#23764=CARTESIAN_POINT('Ctrl Pts',(6.56268467750003,38.2492500034685,-5.80515448811441));
#23765=CARTESIAN_POINT('Ctrl Pts',(5.3093234328217,38.1222500034686,-4.08005073111972));
#23766=CARTESIAN_POINT('Ctrl Pts',(4.05596218814312,37.9952500034685,-2.35494697412514));
#23767=CARTESIAN_POINT('Ctrl Pts',(2.0279810940716,37.8682500034686,-1.69601597307323));
#23768=CARTESIAN_POINT('Ctrl Pts',(0.,37.7412500034685,-1.0370849720215));
#23769=CARTESIAN_POINT('Ctrl Pts',(-2.02798109407148,37.6142500034686,-1.69601597307323));
#23770=CARTESIAN_POINT('Ctrl Pts',(-4.05596218814312,37.4872500034686,-2.35494697412514));
#23771=CARTESIAN_POINT('Ctrl Pts',(-5.30932343282153,37.3602500034685,-4.08005073111972));
#23772=CARTESIAN_POINT('Ctrl Pts',(-6.56268467749997,37.2332500034686,-5.80515448811441));
#23773=CARTESIAN_POINT('Ctrl Pts',(-6.56268467749999,37.1062500034686,-7.93750000000004));
#23774=CARTESIAN_POINT('Ctrl Pts',(-6.56268467749997,36.9792500034686,-10.0698455118856));
#23775=CARTESIAN_POINT('Ctrl Pts',(-5.30932343282153,36.8522500034686,-11.7949492688803));
#23776=CARTESIAN_POINT('Ctrl Pts',(-4.05596218814306,36.7252500034685,-13.5200530258749));
#23777=CARTESIAN_POINT('Ctrl Pts',(-2.02798109407154,36.5982500034687,-14.1789840269267));
#23778=CARTESIAN_POINT('Ctrl Pts',(1.1673575708729E-13,36.4712500034686,
-14.8379150279786));
#23779=CARTESIAN_POINT('Ctrl Pts',(2.02798109407154,36.3442500034687,-14.1789840269267));
#23780=CARTESIAN_POINT('Ctrl Pts',(4.05596218814324,36.2172500034686,-13.5200530258749));
#23781=CARTESIAN_POINT('Ctrl Pts',(5.30932343282164,36.0902500034686,-11.7949492688803));
#23782=CARTESIAN_POINT('Ctrl Pts',(6.56268467750008,35.9632500034686,-10.0698455118856));
#23783=CARTESIAN_POINT('Ctrl Pts',(6.56268467749999,35.8362500034687,-7.93750000000004));
#23784=CARTESIAN_POINT('Origin',(-2.53888687851145E-9,74.888750003468,-7.9374999999999));
#23785=CARTESIAN_POINT('',(6.56268467750004,32.6612500034686,-7.93750000007101));
#23786=CARTESIAN_POINT('',(6.56268467750004,33.2962500034686,-7.93750000006994));
#23787=CARTESIAN_POINT('',(6.56268467242224,74.8887500034674,-7.93749999999981));
#23788=CARTESIAN_POINT('Ctrl Pts',(6.56268467749999,35.2012500034686,-7.93750000000004));
#23789=CARTESIAN_POINT('Ctrl Pts',(6.56268467749997,35.0742500034685,-5.80515448811441));
#23790=CARTESIAN_POINT('Ctrl Pts',(5.30932343282159,34.9472500034685,-4.08005073111972));
#23791=CARTESIAN_POINT('Ctrl Pts',(4.05596218814318,34.8202500034686,-2.35494697412514));
#23792=CARTESIAN_POINT('Ctrl Pts',(2.0279810940716,34.6932500034686,-1.69601597307323));
#23793=CARTESIAN_POINT('Ctrl Pts',(0.,34.5662500034686,-1.0370849720215));
#23794=CARTESIAN_POINT('Ctrl Pts',(-2.0279810940716,34.4392500034686,-1.69601597307323));
#23795=CARTESIAN_POINT('Ctrl Pts',(-4.05596218814318,34.3122500034686,-2.35494697412514));
#23796=CARTESIAN_POINT('Ctrl Pts',(-5.30932343282153,34.1852500034686,-4.08005073111972));
#23797=CARTESIAN_POINT('Ctrl Pts',(-6.56268467749997,34.0582500034686,-5.80515448811441));
#23798=CARTESIAN_POINT('Ctrl Pts',(-6.56268467749999,33.9312500034686,-7.93750000000004));
#23799=CARTESIAN_POINT('Ctrl Pts',(-6.56268467750003,33.8042500034686,-10.0698455118856));
#23800=CARTESIAN_POINT('Ctrl Pts',(-5.30932343282148,33.6772500034685,-11.7949492688803));
#23801=CARTESIAN_POINT('Ctrl Pts',(-4.05596218814306,33.5502500034685,-13.5200530258749));
#23802=CARTESIAN_POINT('Ctrl Pts',(-2.02798109407154,33.4232500034688,-14.1789840269267));
#23803=CARTESIAN_POINT('Ctrl Pts',(0.,33.2962500034685,-14.8379150279786));
#23804=CARTESIAN_POINT('Ctrl Pts',(2.02798109407165,33.1692500034688,-14.1789840269267));
#23805=CARTESIAN_POINT('Ctrl Pts',(4.05596218814318,33.0422500034686,-13.5200530258749));
#23806=CARTESIAN_POINT('Ctrl Pts',(5.30932343282159,32.9152500034686,-11.7949492688803));
#23807=CARTESIAN_POINT('Ctrl Pts',(6.56268467750003,32.7882500034685,-10.0698455118856));
#23808=CARTESIAN_POINT('Ctrl Pts',(6.56268467750004,32.6612500034686,-7.93750000000004));
#23809=CARTESIAN_POINT('Ctrl Pts',(6.56268467749999,35.8362500034687,-7.93750000000004));
#23810=CARTESIAN_POINT('Ctrl Pts',(6.56268467750003,35.7092500034686,-5.80515448811441));
#23811=CARTESIAN_POINT('Ctrl Pts',(5.30932343282159,35.5822500034686,-4.08005073111972));
#23812=CARTESIAN_POINT('Ctrl Pts',(4.05596218814312,35.4552500034686,-2.35494697412514));
#23813=CARTESIAN_POINT('Ctrl Pts',(2.0279810940716,35.3282500034686,-1.69601597307323));
#23814=CARTESIAN_POINT('Ctrl Pts',(5.83678785436452E-14,35.2012500034686,
-1.0370849720215));
#23815=CARTESIAN_POINT('Ctrl Pts',(-2.02798109407148,35.0742500034686,-1.69601597307323));
#23816=CARTESIAN_POINT('Ctrl Pts',(-4.05596218814312,34.9472500034686,-2.35494697412514));
#23817=CARTESIAN_POINT('Ctrl Pts',(-5.30932343282153,34.8202500034686,-4.08005073111972));
#23818=CARTESIAN_POINT('Ctrl Pts',(-6.56268467750003,34.6932500034686,-5.80515448811441));
#23819=CARTESIAN_POINT('Ctrl Pts',(-6.56268467749999,34.5662500034686,-7.93750000000004));
#23820=CARTESIAN_POINT('Ctrl Pts',(-6.56268467749997,34.4392500034686,-10.0698455118856));
#23821=CARTESIAN_POINT('Ctrl Pts',(-5.30932343282148,34.3122500034686,-11.7949492688803));
#23822=CARTESIAN_POINT('Ctrl Pts',(-4.05596218814312,34.1852500034684,-13.5200530258749));
#23823=CARTESIAN_POINT('Ctrl Pts',(-2.02798109407154,34.0582500034686,-14.1789840269267));
#23824=CARTESIAN_POINT('Ctrl Pts',(0.,33.9312500034685,-14.8379150279786));
#23825=CARTESIAN_POINT('Ctrl Pts',(2.0279810940716,33.8042500034687,-14.1789840269267));
#23826=CARTESIAN_POINT('Ctrl Pts',(4.05596218814312,33.6772500034686,-13.5200530258749));
#23827=CARTESIAN_POINT('Ctrl Pts',(5.30932343282164,33.5502500034686,-11.7949492688803));
#23828=CARTESIAN_POINT('Ctrl Pts',(6.56268467750008,33.4232500034685,-10.0698455118856));
#23829=CARTESIAN_POINT('Ctrl Pts',(6.56268467750004,33.2962500034686,-7.93750000000004));
#23830=CARTESIAN_POINT('Origin',(-2.53888687851145E-9,74.888750003468,-7.9374999999999));
#23831=CARTESIAN_POINT('',(6.5626846775001,30.1212500034686,-7.93750000007529));
#23832=CARTESIAN_POINT('',(6.56268467750004,30.7562500034686,-7.93750000007422));
#23833=CARTESIAN_POINT('',(6.56268467242224,74.8887500034674,-7.93749999999981));
#23834=CARTESIAN_POINT('Ctrl Pts',(6.56268467750004,32.6612500034686,-7.93750000000004));
#23835=CARTESIAN_POINT('Ctrl Pts',(6.56268467750008,32.5342500034685,-5.80515448811441));
#23836=CARTESIAN_POINT('Ctrl Pts',(5.30932343282159,32.4072500034686,-4.08005073111972));
#23837=CARTESIAN_POINT('Ctrl Pts',(4.05596218814318,32.2802500034685,-2.35494697412514));
#23838=CARTESIAN_POINT('Ctrl Pts',(2.02798109407165,32.1532500034687,-1.69601597307323));
#23839=CARTESIAN_POINT('Ctrl Pts',(0.,32.0262500034685,-1.0370849720215));
#23840=CARTESIAN_POINT('Ctrl Pts',(-2.02798109407154,31.8992500034685,-1.69601597307323));
#23841=CARTESIAN_POINT('Ctrl Pts',(-4.05596218814318,31.7722500034685,-2.35494697412514));
#23842=CARTESIAN_POINT('Ctrl Pts',(-5.30932343282148,31.6452500034686,-4.08005073111972));
#23843=CARTESIAN_POINT('Ctrl Pts',(-6.56268467749997,31.5182500034685,-5.80515448811441));
#23844=CARTESIAN_POINT('Ctrl Pts',(-6.56268467749999,31.3912500034687,-7.93750000000004));
#23845=CARTESIAN_POINT('Ctrl Pts',(-6.56268467750003,31.2642500034685,-10.0698455118856));
#23846=CARTESIAN_POINT('Ctrl Pts',(-5.30932343282148,31.1372500034686,-11.7949492688803));
#23847=CARTESIAN_POINT('Ctrl Pts',(-4.05596218814318,31.0102500034686,-13.5200530258749));
#23848=CARTESIAN_POINT('Ctrl Pts',(-2.0279810940716,30.8832500034687,-14.1789840269267));
#23849=CARTESIAN_POINT('Ctrl Pts',(0.,30.7562500034685,-14.8379150279786));
#23850=CARTESIAN_POINT('Ctrl Pts',(2.0279810940716,30.6292500034687,-14.1789840269267));
#23851=CARTESIAN_POINT('Ctrl Pts',(4.05596218814312,30.5022500034686,-13.5200530258749));
#23852=CARTESIAN_POINT('Ctrl Pts',(5.30932343282159,30.3752500034686,-11.7949492688803));
#23853=CARTESIAN_POINT('Ctrl Pts',(6.56268467750003,30.2482500034686,-10.0698455118856));
#23854=CARTESIAN_POINT('Ctrl Pts',(6.5626846775001,30.1212500034686,-7.93750000000004));
#23855=CARTESIAN_POINT('Ctrl Pts',(6.56268467750004,33.2962500034686,-7.93750000000004));
#23856=CARTESIAN_POINT('Ctrl Pts',(6.56268467749991,33.1692500034685,-5.80515448811441));
#23857=CARTESIAN_POINT('Ctrl Pts',(5.30932343282159,33.0422500034686,-4.08005073111972));
#23858=CARTESIAN_POINT('Ctrl Pts',(4.05596218814324,32.9152500034685,-2.35494697412514));
#23859=CARTESIAN_POINT('Ctrl Pts',(2.02798109407165,32.7882500034686,-1.69601597307323));
#23860=CARTESIAN_POINT('Ctrl Pts',(0.,32.6612500034685,-1.0370849720215));
#23861=CARTESIAN_POINT('Ctrl Pts',(-2.02798109407154,32.5342500034686,-1.69601597307323));
#23862=CARTESIAN_POINT('Ctrl Pts',(-4.05596218814312,32.4072500034686,-2.35494697412514));
#23863=CARTESIAN_POINT('Ctrl Pts',(-5.30932343282148,32.2802500034686,-4.08005073111972));
#23864=CARTESIAN_POINT('Ctrl Pts',(-6.56268467749991,32.1532500034685,-5.80515448811441));
#23865=CARTESIAN_POINT('Ctrl Pts',(-6.56268467749999,32.0262500034685,-7.93750000000004));
#23866=CARTESIAN_POINT('Ctrl Pts',(-6.56268467749997,31.8992500034685,-10.0698455118856));
#23867=CARTESIAN_POINT('Ctrl Pts',(-5.30932343282159,31.7722500034686,-11.7949492688803));
#23868=CARTESIAN_POINT('Ctrl Pts',(-4.05596218814312,31.6452500034686,-13.5200530258749));
#23869=CARTESIAN_POINT('Ctrl Pts',(-2.02798109407148,31.5182500034687,-14.1789840269267));
#23870=CARTESIAN_POINT('Ctrl Pts',(0.,31.3912500034685,-14.8379150279786));
#23871=CARTESIAN_POINT('Ctrl Pts',(2.0279810940716,31.2642500034687,-14.1789840269267));
#23872=CARTESIAN_POINT('Ctrl Pts',(4.05596218814312,31.1372500034686,-13.5200530258749));
#23873=CARTESIAN_POINT('Ctrl Pts',(5.30932343282159,31.0102500034686,-11.7949492688803));
#23874=CARTESIAN_POINT('Ctrl Pts',(6.56268467749997,30.8832500034686,-10.0698455118856));
#23875=CARTESIAN_POINT('Ctrl Pts',(6.56268467750004,30.7562500034686,-7.93750000000004));
#23876=CARTESIAN_POINT('Origin',(-2.53888687851145E-9,74.888750003468,-7.9374999999999));
#23877=CARTESIAN_POINT('',(6.5626846775001,27.5812500034686,-7.93750000007956));
#23878=CARTESIAN_POINT('',(6.56268467749999,28.2162500034686,-7.93750000007849));
#23879=CARTESIAN_POINT('',(6.56268467242224,74.8887500034674,-7.93749999999981));
#23880=CARTESIAN_POINT('Ctrl Pts',(6.5626846775001,30.1212500034686,-7.93750000000004));
#23881=CARTESIAN_POINT('Ctrl Pts',(6.56268467750003,29.9942500034686,-5.80515448811441));
#23882=CARTESIAN_POINT('Ctrl Pts',(5.30932343282159,29.8672500034686,-4.08005073111972));
#23883=CARTESIAN_POINT('Ctrl Pts',(4.05596218814318,29.7402500034686,-2.35494697412514));
#23884=CARTESIAN_POINT('Ctrl Pts',(2.02798109407165,29.6132500034686,-1.69601597307323));
#23885=CARTESIAN_POINT('Ctrl Pts',(0.,29.4862500034686,-1.0370849720215));
#23886=CARTESIAN_POINT('Ctrl Pts',(-2.02798109407154,29.3592500034686,-1.69601597307323));
#23887=CARTESIAN_POINT('Ctrl Pts',(-4.05596218814312,29.2322500034686,-2.35494697412503));
#23888=CARTESIAN_POINT('Ctrl Pts',(-5.30932343282159,29.1052500034686,-4.08005073111972));
#23889=CARTESIAN_POINT('Ctrl Pts',(-6.56268467749997,28.9782500034685,-5.80515448811441));
#23890=CARTESIAN_POINT('Ctrl Pts',(-6.56268467749993,28.8512500034686,-7.93750000000004));
#23891=CARTESIAN_POINT('Ctrl Pts',(-6.56268467750003,28.7242500034685,-10.0698455118856));
#23892=CARTESIAN_POINT('Ctrl Pts',(-5.30932343282159,28.5972500034687,-11.7949492688803));
#23893=CARTESIAN_POINT('Ctrl Pts',(-4.05596218814306,28.4702500034686,-13.5200530258749));
#23894=CARTESIAN_POINT('Ctrl Pts',(-2.0279810940716,28.3432500034687,-14.1789840269267));
#23895=CARTESIAN_POINT('Ctrl Pts',(1.1673575708729E-13,28.2162500034685,
-14.8379150279786));
#23896=CARTESIAN_POINT('Ctrl Pts',(2.0279810940716,28.0892500034687,-14.1789840269267));
#23897=CARTESIAN_POINT('Ctrl Pts',(4.05596218814324,27.9622500034685,-13.5200530258749));
#23898=CARTESIAN_POINT('Ctrl Pts',(5.30932343282159,27.8352500034685,-11.7949492688803));
#23899=CARTESIAN_POINT('Ctrl Pts',(6.56268467750003,27.7082500034685,-10.0698455118856));
#23900=CARTESIAN_POINT('Ctrl Pts',(6.5626846775001,27.5812500034686,-7.93750000000004));
#23901=CARTESIAN_POINT('Ctrl Pts',(6.56268467750004,30.7562500034686,-7.93750000000004));
#23902=CARTESIAN_POINT('Ctrl Pts',(6.56268467750003,30.6292500034685,-5.80515448811441));
#23903=CARTESIAN_POINT('Ctrl Pts',(5.30932343282159,30.5022500034686,-4.08005073111972));
#23904=CARTESIAN_POINT('Ctrl Pts',(4.05596218814312,30.3752500034686,-2.35494697412514));
#23905=CARTESIAN_POINT('Ctrl Pts',(2.02798109407154,30.2482500034685,-1.69601597307323));
#23906=CARTESIAN_POINT('Ctrl Pts',(0.,30.1212500034685,-1.0370849720215));
#23907=CARTESIAN_POINT('Ctrl Pts',(-2.02798109407154,29.9942500034686,-1.69601597307323));
#23908=CARTESIAN_POINT('Ctrl Pts',(-4.05596218814312,29.8672500034686,-2.35494697412503));
#23909=CARTESIAN_POINT('Ctrl Pts',(-5.30932343282148,29.7402500034687,-4.08005073111972));
#23910=CARTESIAN_POINT('Ctrl Pts',(-6.56268467750003,29.6132500034685,-5.80515448811441));
#23911=CARTESIAN_POINT('Ctrl Pts',(-6.56268467749993,29.4862500034685,-7.93750000000004));
#23912=CARTESIAN_POINT('Ctrl Pts',(-6.56268467749997,29.3592500034685,-10.0698455118856));
#23913=CARTESIAN_POINT('Ctrl Pts',(-5.30932343282159,29.2322500034685,-11.7949492688803));
#23914=CARTESIAN_POINT('Ctrl Pts',(-4.05596218814312,29.1052500034686,-13.5200530258749));
#23915=CARTESIAN_POINT('Ctrl Pts',(-2.02798109407148,28.9782500034687,-14.1789840269267));
#23916=CARTESIAN_POINT('Ctrl Pts',(0.,28.8512500034685,-14.8379150279786));
#23917=CARTESIAN_POINT('Ctrl Pts',(2.0279810940716,28.7242500034687,-14.1789840269267));
#23918=CARTESIAN_POINT('Ctrl Pts',(4.05596218814318,28.5972500034685,-13.5200530258749));
#23919=CARTESIAN_POINT('Ctrl Pts',(5.30932343282159,28.4702500034686,-11.7949492688803));
#23920=CARTESIAN_POINT('Ctrl Pts',(6.56268467750008,28.3432500034685,-10.0698455118856));
#23921=CARTESIAN_POINT('Ctrl Pts',(6.56268467749999,28.2162500034686,-7.93750000000004));
#23922=CARTESIAN_POINT('Origin',(-2.53888687851145E-9,74.888750003468,-7.9374999999999));
#23923=CARTESIAN_POINT('',(6.5626846775001,25.0412500034685,-7.93750000008384));
#23924=CARTESIAN_POINT('',(6.56268467749999,25.6762500034685,-7.93750000008277));
#23925=CARTESIAN_POINT('',(6.56268467242224,74.8887500034674,-7.93749999999981));
#23926=CARTESIAN_POINT('Ctrl Pts',(6.5626846775001,27.5812500034686,-7.93750000000004));
#23927=CARTESIAN_POINT('Ctrl Pts',(6.56268467750003,27.4542500034686,-5.80515448811441));
#23928=CARTESIAN_POINT('Ctrl Pts',(5.30932343282153,27.3272500034686,-4.08005073111972));
#23929=CARTESIAN_POINT('Ctrl Pts',(4.05596218814312,27.2002500034686,-2.35494697412514));
#23930=CARTESIAN_POINT('Ctrl Pts',(2.02798109407165,27.0732500034686,-1.69601597307323));
#23931=CARTESIAN_POINT('Ctrl Pts',(1.1673575708729E-13,26.9462500034685,
-1.0370849720215));
#23932=CARTESIAN_POINT('Ctrl Pts',(-2.02798109407148,26.8192500034686,-1.69601597307323));
#23933=CARTESIAN_POINT('Ctrl Pts',(-4.05596218814312,26.6922500034685,-2.35494697412503));
#23934=CARTESIAN_POINT('Ctrl Pts',(-5.30932343282159,26.5652500034685,-4.08005073111972));
#23935=CARTESIAN_POINT('Ctrl Pts',(-6.56268467750008,26.4382500034685,-5.80515448811441));
#23936=CARTESIAN_POINT('Ctrl Pts',(-6.56268467750004,26.3112500034686,-7.93750000000004));
#23937=CARTESIAN_POINT('Ctrl Pts',(-6.56268467749997,26.1842500034686,-10.0698455118856));
#23938=CARTESIAN_POINT('Ctrl Pts',(-5.30932343282159,26.0572500034686,-11.7949492688803));
#23939=CARTESIAN_POINT('Ctrl Pts',(-4.05596218814318,25.9302500034685,-13.5200530258749));
#23940=CARTESIAN_POINT('Ctrl Pts',(-2.0279810940716,25.8032500034687,-14.1789840269267));
#23941=CARTESIAN_POINT('Ctrl Pts',(0.,25.6762500034686,-14.8379150279786));
#23942=CARTESIAN_POINT('Ctrl Pts',(2.02798109407165,25.5492500034687,-14.1789840269267));
#23943=CARTESIAN_POINT('Ctrl Pts',(4.05596218814312,25.4222500034686,-13.5200530258749));
#23944=CARTESIAN_POINT('Ctrl Pts',(5.30932343282153,25.2952500034686,-11.7949492688803));
#23945=CARTESIAN_POINT('Ctrl Pts',(6.56268467750008,25.1682500034686,-10.0698455118856));
#23946=CARTESIAN_POINT('Ctrl Pts',(6.5626846775001,25.0412500034685,-7.93750000000004));
#23947=CARTESIAN_POINT('Ctrl Pts',(6.56268467749999,28.2162500034686,-7.93750000000004));
#23948=CARTESIAN_POINT('Ctrl Pts',(6.56268467749997,28.0892500034686,-5.80515448811441));
#23949=CARTESIAN_POINT('Ctrl Pts',(5.30932343282164,27.9622500034686,-4.08005073111972));
#23950=CARTESIAN_POINT('Ctrl Pts',(4.05596218814312,27.8352500034686,-2.35494697412514));
#23951=CARTESIAN_POINT('Ctrl Pts',(2.02798109407154,27.7082500034687,-1.69601597307323));
#23952=CARTESIAN_POINT('Ctrl Pts',(0.,27.5812500034685,-1.0370849720215));
#23953=CARTESIAN_POINT('Ctrl Pts',(-2.02798109407148,27.4542500034686,-1.69601597307323));
#23954=CARTESIAN_POINT('Ctrl Pts',(-4.05596218814312,27.3272500034686,-2.35494697412503));
#23955=CARTESIAN_POINT('Ctrl Pts',(-5.30932343282159,27.2002500034686,-4.08005073111972));
#23956=CARTESIAN_POINT('Ctrl Pts',(-6.56268467750003,27.0732500034685,-5.80515448811441));
#23957=CARTESIAN_POINT('Ctrl Pts',(-6.56268467749993,26.9462500034687,-7.93750000000004));
#23958=CARTESIAN_POINT('Ctrl Pts',(-6.56268467749991,26.8192500034686,-10.0698455118856));
#23959=CARTESIAN_POINT('Ctrl Pts',(-5.30932343282159,26.6922500034685,-11.7949492688803));
#23960=CARTESIAN_POINT('Ctrl Pts',(-4.05596218814312,26.5652500034685,-13.5200530258749));
#23961=CARTESIAN_POINT('Ctrl Pts',(-2.02798109407148,26.4382500034687,-14.1789840269267));
#23962=CARTESIAN_POINT('Ctrl Pts',(0.,26.3112500034686,-14.8379150279786));
#23963=CARTESIAN_POINT('Ctrl Pts',(2.02798109407165,26.1842500034687,-14.1789840269267));
#23964=CARTESIAN_POINT('Ctrl Pts',(4.05596218814318,26.0572500034686,-13.5200530258749));
#23965=CARTESIAN_POINT('Ctrl Pts',(5.30932343282159,25.9302500034686,-11.7949492688803));
#23966=CARTESIAN_POINT('Ctrl Pts',(6.56268467750003,25.8032500034686,-10.0698455118856));
#23967=CARTESIAN_POINT('Ctrl Pts',(6.56268467749999,25.6762500034685,-7.93750000000004));
#23968=CARTESIAN_POINT('Origin',(-2.53888687851145E-9,74.888750003468,-7.9374999999999));
#23969=CARTESIAN_POINT('',(6.5626846775001,22.5012500034686,-7.93750000008812));
#23970=CARTESIAN_POINT('',(6.56268467749999,23.1362500034686,-7.93750000008705));
#23971=CARTESIAN_POINT('',(6.56268467242224,74.8887500034674,-7.93749999999981));
#23972=CARTESIAN_POINT('Ctrl Pts',(6.5626846775001,25.0412500034685,-7.93750000000004));
#23973=CARTESIAN_POINT('Ctrl Pts',(6.56268467750003,24.9142500034686,-5.80515448811441));
#23974=CARTESIAN_POINT('Ctrl Pts',(5.30932343282153,24.7872500034686,-4.08005073111972));
#23975=CARTESIAN_POINT('Ctrl Pts',(4.05596218814324,24.6602500034686,-2.35494697412514));
#23976=CARTESIAN_POINT('Ctrl Pts',(2.02798109407171,24.5332500034686,-1.69601597307323));
#23977=CARTESIAN_POINT('Ctrl Pts',(0.,24.4062500034686,-1.0370849720215));
#23978=CARTESIAN_POINT('Ctrl Pts',(-2.0279810940716,24.2792500034685,-1.69601597307323));
#23979=CARTESIAN_POINT('Ctrl Pts',(-4.05596218814312,24.1522500034685,-2.35494697412503));
#23980=CARTESIAN_POINT('Ctrl Pts',(-5.30932343282159,24.0252500034685,-4.08005073111972));
#23981=CARTESIAN_POINT('Ctrl Pts',(-6.56268467749991,23.8982500034686,-5.80515448811441));
#23982=CARTESIAN_POINT('Ctrl Pts',(-6.56268467749999,23.7712500034686,-7.93750000000004));
#23983=CARTESIAN_POINT('Ctrl Pts',(-6.56268467749997,23.6442500034686,-10.0698455118856));
#23984=CARTESIAN_POINT('Ctrl Pts',(-5.30932343282164,23.5172500034686,-11.7949492688803));
#23985=CARTESIAN_POINT('Ctrl Pts',(-4.05596218814312,23.3902500034686,-13.5200530258749));
#23986=CARTESIAN_POINT('Ctrl Pts',(-2.02798109407154,23.2632500034686,-14.1789840269267));
#23987=CARTESIAN_POINT('Ctrl Pts',(0.,23.1362500034685,-14.8379150279786));
#23988=CARTESIAN_POINT('Ctrl Pts',(2.02798109407165,23.0092500034686,-14.1789840269267));
#23989=CARTESIAN_POINT('Ctrl Pts',(4.05596218814312,22.8822500034685,-13.5200530258749));
#23990=CARTESIAN_POINT('Ctrl Pts',(5.30932343282153,22.7552500034686,-11.7949492688803));
#23991=CARTESIAN_POINT('Ctrl Pts',(6.56268467749997,22.6282500034686,-10.0698455118856));
#23992=CARTESIAN_POINT('Ctrl Pts',(6.5626846775001,22.5012500034686,-7.93750000000004));
#23993=CARTESIAN_POINT('Ctrl Pts',(6.56268467749999,25.6762500034685,-7.93750000000004));
#23994=CARTESIAN_POINT('Ctrl Pts',(6.56268467749997,25.5492500034686,-5.80515448811441));
#23995=CARTESIAN_POINT('Ctrl Pts',(5.30932343282164,25.4222500034686,-4.08005073111972));
#23996=CARTESIAN_POINT('Ctrl Pts',(4.05596218814312,25.2952500034686,-2.35494697412514));
#23997=CARTESIAN_POINT('Ctrl Pts',(2.0279810940716,25.1682500034687,-1.69601597307323));
#23998=CARTESIAN_POINT('Ctrl Pts',(0.,25.0412500034686,-1.0370849720215));
#23999=CARTESIAN_POINT('Ctrl Pts',(-2.02798109407148,24.9142500034685,-1.69601597307323));
#24000=CARTESIAN_POINT('Ctrl Pts',(-4.05596218814318,24.7872500034685,-2.35494697412503));
#24001=CARTESIAN_POINT('Ctrl Pts',(-5.30932343282159,24.6602500034686,-4.08005073111972));
#24002=CARTESIAN_POINT('Ctrl Pts',(-6.56268467750003,24.5332500034686,-5.80515448811441));
#24003=CARTESIAN_POINT('Ctrl Pts',(-6.56268467749987,24.4062500034686,-7.93750000000004));
#24004=CARTESIAN_POINT('Ctrl Pts',(-6.56268467750003,24.2792500034686,-10.0698455118856));
#24005=CARTESIAN_POINT('Ctrl Pts',(-5.30932343282153,24.1522500034687,-11.7949492688803));
#24006=CARTESIAN_POINT('Ctrl Pts',(-4.05596218814324,24.0252500034686,-13.5200530258749));
#24007=CARTESIAN_POINT('Ctrl Pts',(-2.02798109407154,23.8982500034687,-14.1789840269267));
#24008=CARTESIAN_POINT('Ctrl Pts',(0.,23.7712500034685,-14.8379150279786));
#24009=CARTESIAN_POINT('Ctrl Pts',(2.02798109407154,23.6442500034687,-14.1789840269267));
#24010=CARTESIAN_POINT('Ctrl Pts',(4.05596218814318,23.5172500034685,-13.5200530258749));
#24011=CARTESIAN_POINT('Ctrl Pts',(5.30932343282164,23.3902500034686,-11.7949492688803));
#24012=CARTESIAN_POINT('Ctrl Pts',(6.56268467750003,23.2632500034686,-10.0698455118856));
#24013=CARTESIAN_POINT('Ctrl Pts',(6.56268467749999,23.1362500034686,-7.93750000000004));
#24014=CARTESIAN_POINT('Origin',(-2.53888687851145E-9,74.888750003468,-7.9374999999999));
#24015=CARTESIAN_POINT('',(6.56268467749999,19.9612500034686,-7.93750000009239));
#24016=CARTESIAN_POINT('',(6.56268467749999,20.5962500034686,-7.93750000009132));
#24017=CARTESIAN_POINT('',(6.56268467242224,74.8887500034674,-7.93749999999981));
#24018=CARTESIAN_POINT('Ctrl Pts',(6.5626846775001,22.5012500034686,-7.93750000000004));
#24019=CARTESIAN_POINT('Ctrl Pts',(6.56268467750003,22.3742500034686,-5.80515448811441));
#24020=CARTESIAN_POINT('Ctrl Pts',(5.30932343282159,22.2472500034686,-4.08005073111972));
#24021=CARTESIAN_POINT('Ctrl Pts',(4.05596218814312,22.1202500034686,-2.35494697412503));
#24022=CARTESIAN_POINT('Ctrl Pts',(2.0279810940716,21.9932500034685,-1.69601597307323));
#24023=CARTESIAN_POINT('Ctrl Pts',(0.,21.8662500034686,-1.0370849720215));
#24024=CARTESIAN_POINT('Ctrl Pts',(-2.0279810940716,21.7392500034686,-1.69601597307323));
#24025=CARTESIAN_POINT('Ctrl Pts',(-4.05596218814312,21.6122500034686,-2.35494697412503));
#24026=CARTESIAN_POINT('Ctrl Pts',(-5.30932343282153,21.4852500034687,-4.08005073111972));
#24027=CARTESIAN_POINT('Ctrl Pts',(-6.56268467750003,21.3582500034686,-5.80515448811441));
#24028=CARTESIAN_POINT('Ctrl Pts',(-6.56268467749999,21.2312500034685,-7.93750000000004));
#24029=CARTESIAN_POINT('Ctrl Pts',(-6.56268467749997,21.1042500034685,-10.0698455118856));
#24030=CARTESIAN_POINT('Ctrl Pts',(-5.30932343282164,20.9772500034686,-11.7949492688803));
#24031=CARTESIAN_POINT('Ctrl Pts',(-4.05596218814312,20.8502500034685,-13.5200530258749));
#24032=CARTESIAN_POINT('Ctrl Pts',(-2.02798109407154,20.7232500034687,-14.1789840269267));
#24033=CARTESIAN_POINT('Ctrl Pts',(0.,20.5962500034686,-14.8379150279786));
#24034=CARTESIAN_POINT('Ctrl Pts',(2.02798109407171,20.4692500034686,-14.1789840269267));
#24035=CARTESIAN_POINT('Ctrl Pts',(4.05596218814324,20.3422500034686,-13.5200530258749));
#24036=CARTESIAN_POINT('Ctrl Pts',(5.30932343282159,20.2152500034686,-11.7949492688803));
#24037=CARTESIAN_POINT('Ctrl Pts',(6.56268467750008,20.0882500034686,-10.0698455118856));
#24038=CARTESIAN_POINT('Ctrl Pts',(6.56268467749999,19.9612500034686,-7.93750000000004));
#24039=CARTESIAN_POINT('Ctrl Pts',(6.56268467749999,23.1362500034686,-7.93750000000004));
#24040=CARTESIAN_POINT('Ctrl Pts',(6.56268467750008,23.0092500034686,-5.80515448811441));
#24041=CARTESIAN_POINT('Ctrl Pts',(5.3093234328217,22.8822500034686,-4.08005073111972));
#24042=CARTESIAN_POINT('Ctrl Pts',(4.05596218814318,22.7552500034685,-2.35494697412503));
#24043=CARTESIAN_POINT('Ctrl Pts',(2.0279810940716,22.6282500034686,-1.69601597307323));
#24044=CARTESIAN_POINT('Ctrl Pts',(-1.1673575708729E-13,22.5012500034685,
-1.0370849720215));
#24045=CARTESIAN_POINT('Ctrl Pts',(-2.02798109407148,22.3742500034686,-1.69601597307323));
#24046=CARTESIAN_POINT('Ctrl Pts',(-4.05596218814306,22.2472500034686,-2.35494697412503));
#24047=CARTESIAN_POINT('Ctrl Pts',(-5.30932343282153,22.1202500034686,-4.08005073111972));
#24048=CARTESIAN_POINT('Ctrl Pts',(-6.56268467749997,21.9932500034685,-5.80515448811441));
#24049=CARTESIAN_POINT('Ctrl Pts',(-6.56268467749987,21.8662500034686,-7.93750000000004));
#24050=CARTESIAN_POINT('Ctrl Pts',(-6.56268467750003,21.7392500034685,-10.0698455118856));
#24051=CARTESIAN_POINT('Ctrl Pts',(-5.30932343282153,21.6122500034686,-11.7949492688803));
#24052=CARTESIAN_POINT('Ctrl Pts',(-4.05596218814318,21.4852500034685,-13.5200530258749));
#24053=CARTESIAN_POINT('Ctrl Pts',(-2.02798109407154,21.3582500034687,-14.1789840269267));
#24054=CARTESIAN_POINT('Ctrl Pts',(0.,21.2312500034686,-14.8379150279786));
#24055=CARTESIAN_POINT('Ctrl Pts',(2.02798109407154,21.1042500034687,-14.1789840269267));
#24056=CARTESIAN_POINT('Ctrl Pts',(4.05596218814312,20.9772500034685,-13.5200530258749));
#24057=CARTESIAN_POINT('Ctrl Pts',(5.30932343282164,20.8502500034686,-11.7949492688803));
#24058=CARTESIAN_POINT('Ctrl Pts',(6.56268467749991,20.7232500034686,-10.0698455118856));
#24059=CARTESIAN_POINT('Ctrl Pts',(6.56268467749999,20.5962500034686,-7.93750000000004));
#24060=CARTESIAN_POINT('Origin',(0.,-18.001,-7.93750000000004));
#24061=CARTESIAN_POINT('',(5.51611152846815E-15,22.3425000069372,-15.875));
#24062=CARTESIAN_POINT('',(-1.63067097993201E-14,22.0250000000001,-15.875));
#24063=CARTESIAN_POINT('',(-9.72063396823211E-16,-18.001,-15.875));
#24064=CARTESIAN_POINT('',(-4.09425652844336E-15,19.8025000069372,-15.875));
#24065=CARTESIAN_POINT('Ctrl Pts',(6.78623823802127E-14,22.3425000069372,
-15.875));
#24066=CARTESIAN_POINT('Ctrl Pts',(0.395040178672521,22.3220459769847,-15.875));
#24067=CARTESIAN_POINT('Ctrl Pts',(0.790420497079234,22.3015743355874,-15.8455096666082));
#24068=CARTESIAN_POINT('Ctrl Pts',(2.1991001059612,22.2286370080217,-15.6332224193839));
#24069=CARTESIAN_POINT('Ctrl Pts',(3.17598716825989,22.1790490668691,-15.2841499417528));
#24070=CARTESIAN_POINT('Ctrl Pts',(4.94518932437667,22.0728978141893,-14.23130929533));
#24071=CARTESIAN_POINT('Ctrl Pts',(5.7200870922735,22.0192899177241,-13.5364058840881));
#24072=CARTESIAN_POINT('Ctrl Pts',(6.97199703691789,21.9162606926934,-11.8741577819405));
#24073=CARTESIAN_POINT('Ctrl Pts',(7.43104000941119,21.8623942176982,-10.9184524179978));
#24074=CARTESIAN_POINT('Ctrl Pts',(7.94396663586668,21.7552586174882,-8.90945821440764));
#24075=CARTESIAN_POINT('Ctrl Pts',(8.00298850093494,21.7056272144354,-7.87818979799516));
#24076=CARTESIAN_POINT('Ctrl Pts',(7.7239878463525,21.6004972097071,-5.8339170308497));
#24077=CARTESIAN_POINT('Ctrl Pts',(7.38230828412897,21.5461497170984,-4.84127477607674));
#24078=CARTESIAN_POINT('Ctrl Pts',(6.33810938427407,21.4411549811571,-3.04837695866961));
#24079=CARTESIAN_POINT('Ctrl Pts',(5.64728214551277,21.3904042997954,-2.26446263971475));
#24080=CARTESIAN_POINT('Ctrl Pts',(4.01126411610705,21.2837505722391,-1.01179935196314));
#24081=CARTESIAN_POINT('Ctrl Pts',(3.08389896379364,21.2321753138586,-0.552044436971875));
#24082=CARTESIAN_POINT('Ctrl Pts',(1.0831538814182,21.128582560383,-0.00460559803268347));
#24083=CARTESIAN_POINT('Ctrl Pts',(0.0266016197439578,21.073877361334,0.0689460350682048));
#24084=CARTESIAN_POINT('Ctrl Pts',(-2.03128985394184,20.9673257341474,-0.196013908491485));
#24085=CARTESIAN_POINT('Ctrl Pts',(-3.0139353749126,20.9178982618204,-0.523126647845116));
#24086=CARTESIAN_POINT('Ctrl Pts',(-4.80649912410774,20.8119606880915,-1.53679171539507));
#24087=CARTESIAN_POINT('Ctrl Pts',(-5.59803512166624,20.7581284717844,-2.21616531313947));
#24088=CARTESIAN_POINT('Ctrl Pts',(-6.88378103002077,20.6545571854372,-3.84965336274376));
#24089=CARTESIAN_POINT('Ctrl Pts',(-7.36182078278323,20.6016562035522,-4.79095067020299));
#24090=CARTESIAN_POINT('Ctrl Pts',(-7.91952396519374,20.4946248469775,-6.78327916318912));
#24091=CARTESIAN_POINT('Ctrl Pts',(-8.00222222662397,20.4446754667674,-7.81281401194153));
#24092=CARTESIAN_POINT('Ctrl Pts',(-7.77007008099423,20.3398966932697,-9.86517616083676));
#24093=CARTESIAN_POINT('Ctrl Pts',(-7.45014540239196,20.2854176146861,-10.8675591854763));
#24094=CARTESIAN_POINT('Ctrl Pts',(-6.44616960099415,20.1799757855807,-12.6826056157578));
#24095=CARTESIAN_POINT('Ctrl Pts',(-5.77523755495239,20.1297467344383,-13.4796773377977));
#24096=CARTESIAN_POINT('Ctrl Pts',(-4.16975728145562,20.0232505572233,-14.7691954209118));
#24097=CARTESIAN_POINT('Ctrl Pts',(-3.25170674616548,19.9708639121129,-15.2508444363837));
#24098=CARTESIAN_POINT('Ctrl Pts',(-1.5302325047701,19.8817309894461,-15.7640055967039));
#24099=CARTESIAN_POINT('Ctrl Pts',(-0.766355811038719,19.8421796789287,
-15.875));
#24100=CARTESIAN_POINT('Ctrl Pts',(1.70696790036118E-14,19.8025000069371,
-15.875));
#24101=CARTESIAN_POINT('',(5.55111512312578E-14,18.0000000000001,-15.875));
#24102=CARTESIAN_POINT('',(-9.72063396823211E-16,-18.001,-15.875));
#24103=CARTESIAN_POINT('',(-4.29373077449685,18.819869818891,-14.6134105960265));
#24104=CARTESIAN_POINT('Ctrl Pts',(-9.72063396823211E-16,18.0000000000001,
-15.875));
#24105=CARTESIAN_POINT('Ctrl Pts',(-0.152276681747816,18.072084637752,-15.875));
#24106=CARTESIAN_POINT('Ctrl Pts',(-0.305855934339734,18.1421428142786,
-15.8706141374141));
#24107=CARTESIAN_POINT('Ctrl Pts',(-0.460325988668671,18.2094023441906,
-15.8616407252873));
#24108=CARTESIAN_POINT('Ctrl Pts',(-0.614082443016771,18.2763511575726,
-15.8527087673229));
#24109=CARTESIAN_POINT('Ctrl Pts',(-0.768721127003723,18.3405271222359,
-15.8392313687975));
#24110=CARTESIAN_POINT('Ctrl Pts',(-0.923815417265365,18.4011687051435,
-15.8210570223614));
#24111=CARTESIAN_POINT('Ctrl Pts',(-0.976648961750814,18.4218265240923,
-15.8148658522074));
#24112=CARTESIAN_POINT('Ctrl Pts',(-1.02953522580605,18.4420741943477,-15.8081300413038));
#24113=CARTESIAN_POINT('Ctrl Pts',(-1.08245691517555,18.4618816114692,-15.80084491656));
#24114=CARTESIAN_POINT('Ctrl Pts',(-1.21556599724492,18.5117013950516,-15.7825213090001));
#24115=CARTESIAN_POINT('Ctrl Pts',(-1.34862695113583,18.5587255077166,-15.7607646847442));
#24116=CARTESIAN_POINT('Ctrl Pts',(-1.4817395657411,18.6025368983511,-15.7354711534038));
#24117=CARTESIAN_POINT('Ctrl Pts',(-1.6130840260593,18.6457663358896,-15.7105135997317));
#24118=CARTESIAN_POINT('Ctrl Pts',(-1.74447921274838,18.6858678346499,-15.6821123226063));
#24119=CARTESIAN_POINT('Ctrl Pts',(-1.87600132923871,18.7224407429927,-15.650121166808));
#24120=CARTESIAN_POINT('Ctrl Pts',(-1.976037833142,18.7502583145603,-15.6257885034714));
#24121=CARTESIAN_POINT('Ctrl Pts',(-2.07614742951161,18.7760345210388,-15.5993780730588));
#24122=CARTESIAN_POINT('Ctrl Pts',(-2.17635351087789,18.7995930649607,-15.5708080407966));
#24123=CARTESIAN_POINT('Ctrl Pts',(-2.27056963336782,18.8217433639203,-15.5439458222321));
#24124=CARTESIAN_POINT('Ctrl Pts',(-2.36523835232703,18.8419415753925,-15.5150640314883));
#24125=CARTESIAN_POINT('Ctrl Pts',(-2.45994739338429,18.8598808531924,-15.4841923265615));
#24126=CARTESIAN_POINT('Ctrl Pts',(-2.55421906742611,18.8777372872817,-15.4534631873845));
#24127=CARTESIAN_POINT('Ctrl Pts',(-2.6485303701587,18.8933556030678,-15.4207624788507));
#24128=CARTESIAN_POINT('Ctrl Pts',(-2.74248535327406,18.9064331858182,-15.3861697025092));
#24129=CARTESIAN_POINT('Ctrl Pts',(-2.83620349346052,18.9194778024299,-15.3516641280828));
#24130=CARTESIAN_POINT('Ctrl Pts',(-2.92956679712358,18.9299944792857,-15.3152760826183));
#24131=CARTESIAN_POINT('Ctrl Pts',(-3.02219766183718,18.9376828843945,-15.2771340196761));
#24132=CARTESIAN_POINT('Ctrl Pts',(-3.10530581747077,18.9445809001944,-15.2429130662931));
#24133=CARTESIAN_POINT('Ctrl Pts',(-3.18782444335918,18.9492022622311,-15.207280908227));
#24134=CARTESIAN_POINT('Ctrl Pts',(-3.26949439648287,18.9513300675967,-15.1703633777618));
#24135=CARTESIAN_POINT('Ctrl Pts',(-3.42087322908613,18.9552740479707,-15.1019351192571));
#24136=CARTESIAN_POINT('Ctrl Pts',(-3.56980099384897,18.9508507374213,-15.0288961392634));
#24137=CARTESIAN_POINT('Ctrl Pts',(-3.71625969440135,18.936539439914,-14.9512949880053));
#24138=CARTESIAN_POINT('Ctrl Pts',(-3.74184003411462,18.9340398420711,-14.9377412434764));
#24139=CARTESIAN_POINT('Ctrl Pts',(-3.76734500463074,18.9312386033842,-14.9240482072849));
#24140=CARTESIAN_POINT('Ctrl Pts',(-3.79277444384613,18.9281276214137,-14.9102159893479));
#24141=CARTESIAN_POINT('Ctrl Pts',(-3.86447430656435,18.9193560170414,-14.8712152029456));
#24142=CARTESIAN_POINT('Ctrl Pts',(-3.93577353808586,18.9080524652382,-14.8309942492684));
#24143=CARTESIAN_POINT('Ctrl Pts',(-4.00627785537239,18.8940495030155,-14.7897729072588));
#24144=CARTESIAN_POINT('Ctrl Pts',(-4.07705725420642,18.8799919064573,-14.7483907349485));
#24145=CARTESIAN_POINT('Ctrl Pts',(-4.1470352971761,18.863213794202,-14.7060004943228));
#24146=CARTESIAN_POINT('Ctrl Pts',(-4.21584055455469,18.8435457354691,-14.6628694819372));
#24147=CARTESIAN_POINT('Ctrl Pts',(-4.24197933063924,18.8360739374871,-14.6464842242113));
#24148=CARTESIAN_POINT('Ctrl Pts',(-4.26794914936831,18.8281850617291,-14.6299925073087));
#24149=CARTESIAN_POINT('Ctrl Pts',(-4.29373077449686,18.819869818891,-14.6134105960265));
#24150=CARTESIAN_POINT('',(-4.29373077449685,18.8198698188908,-1.26158940397347));
#24151=CARTESIAN_POINT('Ctrl Pts',(-4.29373077449685,18.819869818891,-14.6134105960265));
#24152=CARTESIAN_POINT('Ctrl Pts',(-4.52296127969864,18.7459370342071,-14.4659769148109));
#24153=CARTESIAN_POINT('Ctrl Pts',(-4.74196146019457,18.6690215823314,-14.3087480538926));
#24154=CARTESIAN_POINT('Ctrl Pts',(-4.95124940477097,18.5902365316974,-14.1417968955388));
#24155=CARTESIAN_POINT('Ctrl Pts',(-5.16682135147801,18.5090859103801,-13.969832923681));
#24156=CARTESIAN_POINT('Ctrl Pts',(-5.37208902136478,18.4259511228614,-13.7875541699567));
#24157=CARTESIAN_POINT('Ctrl Pts',(-5.56758051682947,18.3420322638492,-13.5950037064242));
#24158=CARTESIAN_POINT('Ctrl Pts',(-5.64332797487214,18.3095160654493,-13.5203958155651));
#24159=CARTESIAN_POINT('Ctrl Pts',(-5.71760730096738,18.2768820318798,-13.4442453974143));
#24160=CARTESIAN_POINT('Ctrl Pts',(-5.79044777763095,18.2441996606711,-13.3665534898537));
#24161=CARTESIAN_POINT('Ctrl Pts',(-5.79212935934825,18.2434451615187,-13.3647599089037));
#24162=CARTESIAN_POINT('Ctrl Pts',(-5.79381016993235,18.2426906385331,-13.3629655109143));
#24163=CARTESIAN_POINT('Ctrl Pts',(-5.79549020982549,18.2419360925352,-13.3611702958253));
#24164=CARTESIAN_POINT('Ctrl Pts',(-5.94895048266734,18.1730134227974,-13.1971895484084));
#24165=CARTESIAN_POINT('Ctrl Pts',(-6.09643741101815,18.1036131389403,-13.0255265848449));
#24166=CARTESIAN_POINT('Ctrl Pts',(-6.23662479546188,18.0350900642456,-12.847493578081));
#24167=CARTESIAN_POINT('Ctrl Pts',(-6.29721400015929,18.0054742852249,-12.7705474367965));
#24168=CARTESIAN_POINT('Ctrl Pts',(-6.35643920688128,17.976022390356,-12.6924109203825));
#24169=CARTESIAN_POINT('Ctrl Pts',(-6.41419086511951,17.9468442552088,-12.6131882492251));
#24170=CARTESIAN_POINT('Ctrl Pts',(-6.41654032136253,17.9456572286563,-12.6099653080141));
#24171=CARTESIAN_POINT('Ctrl Pts',(-6.41888732415843,17.9444706625728,-12.6067405888829));
#24172=CARTESIAN_POINT('Ctrl Pts',(-6.42123186600278,17.9432845644396,-12.6035140991033));
#24173=CARTESIAN_POINT('Ctrl Pts',(-6.56679359836233,17.8696452308427,-12.4031963087054));
#24174=CARTESIAN_POINT('Ctrl Pts',(-6.70230659924676,17.7981518448594,-12.1970951577147));
#24175=CARTESIAN_POINT('Ctrl Pts',(-6.82801702228201,17.7297067509173,-11.9849986789165));
#24176=CARTESIAN_POINT('Ctrl Pts',(-6.86647149527177,17.7087695847482,-11.9201189488333));
#24177=CARTESIAN_POINT('Ctrl Pts',(-6.90400842021663,17.6881177916409,-11.8546780384769));
#24178=CARTESIAN_POINT('Ctrl Pts',(-6.94063408540422,17.6677776026631,-11.7886694036638));
#24179=CARTESIAN_POINT('Ctrl Pts',(-6.94307149280364,17.6664239800909,-11.7842765841997));
#24180=CARTESIAN_POINT('Ctrl Pts',(-6.94550485844196,17.665071741036,-11.7798812608693));
#24181=CARTESIAN_POINT('Ctrl Pts',(-6.94793418394148,17.6637208933711,-11.7754834321708));
#24182=CARTESIAN_POINT('Ctrl Pts',(-7.07457713217915,17.5932999757431,-11.5462206214354));
#24183=CARTESIAN_POINT('Ctrl Pts',(-7.19024425841544,17.5266506308609,-11.3101531082747));
#24184=CARTESIAN_POINT('Ctrl Pts',(-7.29463565879605,17.4650089179132,-11.0667676520206));
#24185=CARTESIAN_POINT('Ctrl Pts',(-7.31828389382657,17.4510449543094,-11.0116324928837));
#24186=CARTESIAN_POINT('Ctrl Pts',(-7.34135334430897,17.4373380947864,-10.956121694965));
#24187=CARTESIAN_POINT('Ctrl Pts',(-7.3638402765716,17.4239029374496,-10.9002291155016));
#24188=CARTESIAN_POINT('Ctrl Pts',(-7.36582071204233,17.4227196963639,-10.8953066278262));
#24189=CARTESIAN_POINT('Ctrl Pts',(-7.36779664658278,17.421538551103,-10.8903811356429));
#24190=CARTESIAN_POINT('Ctrl Pts',(-7.36976807627246,17.4203595125087,-10.8854526373327));
#24191=CARTESIAN_POINT('Ctrl Pts',(-7.44546738546979,17.3750865780631,-10.6962072792993));
#24192=CARTESIAN_POINT('Ctrl Pts',(-7.51472895154413,17.3327859329971,-10.5014874371513));
#24193=CARTESIAN_POINT('Ctrl Pts',(-7.57645236773666,17.29455943516,-10.3039688005431));
#24194=CARTESIAN_POINT('Ctrl Pts',(-7.61348923770643,17.2716217898201,-10.1854485935952));
#24195=CARTESIAN_POINT('Ctrl Pts',(-7.6478123110375,17.2501510470236,-10.0659218717069));
#24196=CARTESIAN_POINT('Ctrl Pts',(-7.67918843644889,17.2303836853404,-9.94597400456573));
#24197=CARTESIAN_POINT('Ctrl Pts',(-7.68031341058551,17.2296749371967,-9.94167333816705));
#24198=CARTESIAN_POINT('Ctrl Pts',(-7.68143460129582,17.2289683741076,-9.93737211336389));
#24199=CARTESIAN_POINT('Ctrl Pts',(-7.682551998173,17.2282640067415,-9.93307035593063));
#24200=CARTESIAN_POINT('Ctrl Pts',(-7.79057552082065,17.1601698088095,-9.51720111465524));
#24201=CARTESIAN_POINT('Ctrl Pts',(-7.86480882869604,17.1119590390803,-9.09494626559864));
#24202=CARTESIAN_POINT('Ctrl Pts',(-7.90422422557617,17.0860934798342,-8.66599267125661));
#24203=CARTESIAN_POINT('Ctrl Pts',(-7.92603246415529,17.07178226311,-8.42865591797634));
#24204=CARTESIAN_POINT('Ctrl Pts',(-7.9371813500848,17.064312408887,-8.1892683562573));
#24205=CARTESIAN_POINT('Ctrl Pts',(-7.93749334978002,17.0641067984408,-7.94777616176066));
#24206=CARTESIAN_POINT('Ctrl Pts',(-7.93749390429189,17.0641064330128,-7.94734696169487));
#24207=CARTESIAN_POINT('Ctrl Pts',(-7.93749442457205,17.0641060905316,-7.94691775513394));
#24208=CARTESIAN_POINT('Ctrl Pts',(-7.93749491061955,17.0641057709997,-7.94648854207958));
#24209=CARTESIAN_POINT('Ctrl Pts',(-7.93768655372469,17.0639797831163,-7.77725462647313));
#24210=CARTESIAN_POINT('Ctrl Pts',(-7.93239900403588,17.0674615298841,-7.60631918039094));
#24211=CARTESIAN_POINT('Ctrl Pts',(-7.92171494756793,17.0744688979786,-7.43716157505265));
#24212=CARTESIAN_POINT('Ctrl Pts',(-7.91102345406276,17.0814811438138,-7.2678862212346));
#24213=CARTESIAN_POINT('Ctrl Pts',(-7.89497393957298,17.0919932010127,-7.09996663012299));
#24214=CARTESIAN_POINT('Ctrl Pts',(-7.87374400759939,17.1058076114062,-6.93347731460257));
#24215=CARTESIAN_POINT('Ctrl Pts',(-7.87346433385428,17.1059895963459,-6.93128405790964));
#24216=CARTESIAN_POINT('Ctrl Pts',(-7.87318376431306,17.1061721542786,-6.92909104881785));
#24217=CARTESIAN_POINT('Ctrl Pts',(-7.87290229918002,17.1063552847221,-6.92689828753272));
#24218=CARTESIAN_POINT('Ctrl Pts',(-7.83036082814314,17.1340341605142,-6.59547787430953));
#24219=CARTESIAN_POINT('Ctrl Pts',(-7.76731445840906,17.174819812098,-6.26939293959585));
#24220=CARTESIAN_POINT('Ctrl Pts',(-7.68426407606719,17.2271865562986,-5.94853246399202));
#24221=CARTESIAN_POINT('Ctrl Pts',(-7.68326626852899,17.2278157157394,-5.9446774907548));
#24222=CARTESIAN_POINT('Ctrl Pts',(-7.68226543432046,17.2284466292013,-5.94082296302115));
#24223=CARTESIAN_POINT('Ctrl Pts',(-7.68126157924107,17.2290792899691,-5.93696889619287));
#24224=CARTESIAN_POINT('Ctrl Pts',(-7.62719229954297,17.2631554357352,-5.72938254075854));
#24225=CARTESIAN_POINT('Ctrl Pts',(-7.56432398380049,17.3023261324512,-5.52301181373151));
#24226=CARTESIAN_POINT('Ctrl Pts',(-7.4935763091711,17.345533282136,-5.32035620488053));
#24227=CARTESIAN_POINT('Ctrl Pts',(-7.45531251771263,17.3689018150767,-5.21075017195316));
#24228=CARTESIAN_POINT('Ctrl Pts',(-7.4147445062259,17.3934507919831,-5.10223040780266));
#24229=CARTESIAN_POINT('Ctrl Pts',(-7.37202153836157,17.4190115694052,-4.99518718727362));
#24230=CARTESIAN_POINT('Ctrl Pts',(-7.37020264317793,17.4200997984602,-4.99062991028669));
#24231=CARTESIAN_POINT('Ctrl Pts',(-7.36837989989909,17.4211898298956,-4.9860752064781));
#24232=CARTESIAN_POINT('Ctrl Pts',(-7.36655331157685,17.422281655205,-4.98152307439258));
#24233=CARTESIAN_POINT('Ctrl Pts',(-7.26791525719856,17.4812415877351,-4.73570224726818));
#24234=CARTESIAN_POINT('Ctrl Pts',(-7.15804389761601,17.5454461273167,-4.49732014145397));
#24235=CARTESIAN_POINT('Ctrl Pts',(-7.03725813864796,17.6136630597091,-4.26584946646392));
#24236=CARTESIAN_POINT('Ctrl Pts',(-7.00830992697048,17.6300123231965,-4.2103738693903));
#24237=CARTESIAN_POINT('Ctrl Pts',(-6.97873464011855,17.6465921971233,-4.1552953738361));
#24238=CARTESIAN_POINT('Ctrl Pts',(-6.94853637755767,17.6633859685258,-4.10060692620219));
#24239=CARTESIAN_POINT('Ctrl Pts',(-6.94626438275752,17.6646494637757,-4.09649238920185));
#24240=CARTESIAN_POINT('Ctrl Pts',(-6.94398886116032,17.6659141722406,-4.09238006080646));
#24241=CARTESIAN_POINT('Ctrl Pts',(-6.94170981151124,17.667180087461,-4.08826993972571));
#24242=CARTESIAN_POINT('Ctrl Pts',(-6.81695592055677,17.7364755718406,-3.86328423249227));
#24243=CARTESIAN_POINT('Ctrl Pts',(-6.68164503357455,17.8093783831497,-3.64493058249314));
#24244=CARTESIAN_POINT('Ctrl Pts',(-6.53553788058789,17.8848500923535,-3.43297205340694));
#24245=CARTESIAN_POINT('Ctrl Pts',(-6.49757915893022,17.9044576854394,-3.37790510668951));
#24246=CARTESIAN_POINT('Ctrl Pts',(-6.45889152043283,17.9242387878716,-3.32326994127638));
#24247=CARTESIAN_POINT('Ctrl Pts',(-6.41947032548397,17.944175414547,-3.26906268219969));
#24248=CARTESIAN_POINT('Ctrl Pts',(-6.26576753847862,18.0219080933118,-3.05770920073322));
#24249=CARTESIAN_POINT('Ctrl Pts',(-6.10302120078014,18.1009132292221,-2.8557968247366));
#24250=CARTESIAN_POINT('Ctrl Pts',(-5.93170231104313,18.1799349593124,-2.66313899571769));
#24251=CARTESIAN_POINT('Ctrl Pts',(-5.88659280047641,18.2007419559838,-2.61241078712826));
#24252=CARTESIAN_POINT('Ctrl Pts',(-5.84088875206301,18.2215501339755,-2.5623244032648));
#24253=CARTESIAN_POINT('Ctrl Pts',(-5.79459835582529,18.2423366010455,-2.51287686611627));
#24254=CARTESIAN_POINT('Ctrl Pts',(-5.79304324259939,18.2430349167327,-2.51121568960325));
#24255=CARTESIAN_POINT('Ctrl Pts',(-5.79148746488087,18.2437332148302,-2.50955520810606));
#24256=CARTESIAN_POINT('Ctrl Pts',(-5.78993102234963,18.2444314946615,-2.50789542163744));
#24257=CARTESIAN_POINT('Ctrl Pts',(-5.60237021560088,18.3285784682036,-2.30788104087095));
#24258=CARTESIAN_POINT('Ctrl Pts',(-5.40518143441788,18.4124500515875,-2.11798146925534));
#24259=CARTESIAN_POINT('Ctrl Pts',(-5.19781723817633,18.4948497478445,-1.93825471385303));
#24260=CARTESIAN_POINT('Ctrl Pts',(-4.9967832052399,18.5747340458648,-1.76401443939882));
#24261=CARTESIAN_POINT('Ctrl Pts',(-4.78618558233977,18.6532355453134,-1.59933547602871));
#24262=CARTESIAN_POINT('Ctrl Pts',(-4.56549139794203,18.7292531909103,-1.44430382682765));
#24263=CARTESIAN_POINT('Ctrl Pts',(-4.47655669487745,18.7598865615054,-1.38182962196841));
#24264=CARTESIAN_POINT('Ctrl Pts',(-4.38598200496235,18.7901164038823,-1.32092242551976));
#24265=CARTESIAN_POINT('Ctrl Pts',(-4.29373077449684,18.8198698188908,-1.2615894039735));
#24266=CARTESIAN_POINT('',(1.11022302462516E-13,18.,0.));
#24267=CARTESIAN_POINT('Ctrl Pts',(-4.29373077449681,18.8198698188908,-1.26158940397354));
#24268=CARTESIAN_POINT('Ctrl Pts',(-4.22582648941137,18.8417707121595,-1.21791555388257));
#24269=CARTESIAN_POINT('Ctrl Pts',(-4.15661453194584,18.86071388632,-1.17487038785831));
#24270=CARTESIAN_POINT('Ctrl Pts',(-4.08645576680373,18.8768690611168,-1.13273802650262));
#24271=CARTESIAN_POINT('Ctrl Pts',(-4.0166014010922,18.8929541430892,-1.09078846578175));
#24272=CARTESIAN_POINT('Ctrl Pts',(-3.9458086305145,18.9062753659277,-1.04974397568514));
#24273=CARTESIAN_POINT('Ctrl Pts',(-3.8744619443222,18.9170002498469,-1.00984160108927));
#24274=CARTESIAN_POINT('Ctrl Pts',(-3.84731136562865,18.9210815438826,-0.99465697767726));
#24275=CARTESIAN_POINT('Ctrl Pts',(-3.82008084867973,18.9247868516778,-0.97963728668364));
#24276=CARTESIAN_POINT('Ctrl Pts',(-3.79279256087207,18.9281254049619,-0.964793865349493));
#24277=CARTESIAN_POINT('Ctrl Pts',(-3.64719779704915,18.945938024073,-0.885597822024888));
#24278=CARTESIAN_POINT('Ctrl Pts',(-3.4991287754235,18.9535969347798,-0.81096042606437));
#24279=CARTESIAN_POINT('Ctrl Pts',(-3.34860693025952,18.952622880884,-0.740921793892792));
#24280=CARTESIAN_POINT('Ctrl Pts',(-3.32232346104453,18.9524527958338,-0.728691952898373));
#24281=CARTESIAN_POINT('Ctrl Pts',(-3.2959651551925,18.9520194863078,-0.716602450005113));
#24282=CARTESIAN_POINT('Ctrl Pts',(-3.26953206999634,18.9513310489586,-0.704653652035405));
#24283=CARTESIAN_POINT('Ctrl Pts',(-3.17850334583775,18.9489602483847,-0.663505075305149));
#24284=CARTESIAN_POINT('Ctrl Pts',(-3.086419875657,18.9434916030851,-0.623954084670512));
#24285=CARTESIAN_POINT('Ctrl Pts',(-2.99364161461572,18.9352254582242,-0.586172491771277));
#24286=CARTESIAN_POINT('Ctrl Pts',(-2.90078198108134,18.9269520634234,-0.548357761988755));
#24287=CARTESIAN_POINT('Ctrl Pts',(-2.80722663233826,18.9158762597357,-0.512315658170322));
#24288=CARTESIAN_POINT('Ctrl Pts',(-2.71335601231357,18.9022991832847,-0.478169909405996));
#24289=CARTESIAN_POINT('Ctrl Pts',(-2.61888384721301,18.8886351017252,-0.443805346629091));
#24290=CARTESIAN_POINT('Ctrl Pts',(-2.52409266754353,18.8724375871946,-0.411361617018201));
#24291=CARTESIAN_POINT('Ctrl Pts',(-2.42938551103078,18.8540136022487,-0.380913979263318));
#24292=CARTESIAN_POINT('Ctrl Pts',(-2.34490238900972,18.8375785636982,-0.353753291619269));
#24293=CARTESIAN_POINT('Ctrl Pts',(-2.26048649576891,18.8193718208331,-0.32818026897181));
#24294=CARTESIAN_POINT('Ctrl Pts',(-2.17643094124134,18.7996112684571,-0.304214036012625));
#24295=CARTESIAN_POINT('Ctrl Pts',(-2.04502170239041,18.7687183767071,-0.266746144104807));
#24296=CARTESIAN_POINT('Ctrl Pts',(-1.91377939287518,18.7340115684466,-0.232990701121492));
#24297=CARTESIAN_POINT('Ctrl Pts',(-1.78264791444894,18.6958884625523,-0.202768416867322));
#24298=CARTESIAN_POINT('Ctrl Pts',(-1.64965288012602,18.657223575694,-0.172116633024579));
#24299=CARTESIAN_POINT('Ctrl Pts',(-1.51677140832459,18.6150446008057,-0.14509896764463));
#24300=CARTESIAN_POINT('Ctrl Pts',(-1.38391902822724,18.5697663509261,-0.121575590609266));
#24301=CARTESIAN_POINT('Ctrl Pts',(-1.28346880481899,18.5355312825546,-0.103789469827784));
#24302=CARTESIAN_POINT('Ctrl Pts',(-1.18303463224986,18.499524379302,-0.088001977634254));
#24303=CARTESIAN_POINT('Ctrl Pts',(-1.08257270443572,18.4619249481095,-0.074171023694225));
#24304=CARTESIAN_POINT('Ctrl Pts',(-0.977468955166084,18.4225882434023,
-0.0597010135450861));
#24305=CARTESIAN_POINT('Ctrl Pts',(-0.872311892508873,18.3814503563709,
-0.0473752902949603));
#24306=CARTESIAN_POINT('Ctrl Pts',(-0.767497582476942,18.3388427147694,
-0.0371928090806906));
#24307=CARTESIAN_POINT('Ctrl Pts',(-0.690645617488946,18.307601933052,-0.0297268085934328));
#24308=CARTESIAN_POINT('Ctrl Pts',(-0.613978042670824,18.2755709939339,
-0.0234119367079837));
#24309=CARTESIAN_POINT('Ctrl Pts',(-0.537651063225293,18.2428805421956,
-0.0182299841328799));
#24310=CARTESIAN_POINT('Ctrl Pts',(-0.45595667868525,18.2078912585309,-0.0126836304134733));
#24311=CARTESIAN_POINT('Ctrl Pts',(-0.374796918314945,18.1722049684806,
-0.00843915814557654));
#24312=CARTESIAN_POINT('Ctrl Pts',(-0.293782657353165,18.1357422451802,
-0.00543860334920243));
#24313=CARTESIAN_POINT('Ctrl Pts',(-0.212550494340367,18.0991814489962,
-0.00242997803491511));
#24314=CARTESIAN_POINT('Ctrl Pts',(-0.131464343433757,18.0618400372384,
-0.000671975325032559));
#24315=CARTESIAN_POINT('Ctrl Pts',(-0.0501289083909383,18.0236379404196,
-0.000158294961541294));
#24316=CARTESIAN_POINT('Ctrl Pts',(-0.0334309211493575,18.0157951333461,
-5.28375043910101E-5));
#24317=CARTESIAN_POINT('Ctrl Pts',(-0.016722425025208,18.0079160508127,
-4.41750233939426E-14));
#24318=CARTESIAN_POINT('Ctrl Pts',(1.11022302462515E-13,18.,-4.44089209850063E-14));
#24319=CARTESIAN_POINT('',(4.29373077449696,18.8198698188909,-1.26158940397347));
#24320=CARTESIAN_POINT('Ctrl Pts',(1.11022302462515E-13,18.,-4.44089209850063E-14));
#24321=CARTESIAN_POINT('Ctrl Pts',(0.152276681653021,18.0720846377099,-4.65388243309537E-14));
#24322=CARTESIAN_POINT('Ctrl Pts',(0.305855934149367,18.1421428141949,-0.0043858625805328));
#24323=CARTESIAN_POINT('Ctrl Pts',(0.460325988382226,18.2094023440686,-0.0133592746961373));
#24324=CARTESIAN_POINT('Ctrl Pts',(0.614082442636275,18.2763511574133,-0.0222912326494619));
#24325=CARTESIAN_POINT('Ctrl Pts',(0.768721126528699,18.3405271220422,-0.0357686311582533));
#24326=CARTESIAN_POINT('Ctrl Pts',(0.923815416695544,18.4011687049212,-0.0539429775719302));
#24327=CARTESIAN_POINT('Ctrl Pts',(0.976648961370601,18.4218265239471,-0.0601341477443072));
#24328=CARTESIAN_POINT('Ctrl Pts',(1.02953522561586,18.4420741942768,-0.0668699586701339));
#24329=CARTESIAN_POINT('Ctrl Pts',(1.08245691517558,18.4618816114694,-0.0741550834401359));
#24330=CARTESIAN_POINT('Ctrl Pts',(1.21556599724415,18.5117013950515,-0.0924786909998602));
#24331=CARTESIAN_POINT('Ctrl Pts',(1.34862695113425,18.5587255077162,-0.114235315255648));
#24332=CARTESIAN_POINT('Ctrl Pts',(1.48173956573871,18.6025368983504,-0.139528846595817));
#24333=CARTESIAN_POINT('Ctrl Pts',(1.61308402605649,18.6457663358888,-0.164486400267772));
#24334=CARTESIAN_POINT('Ctrl Pts',(1.74447921274513,18.685867834649,-0.192887677393095));
#24335=CARTESIAN_POINT('Ctrl Pts',(1.87600132923503,18.7224407429918,-0.224878833191163));
#24336=CARTESIAN_POINT('Ctrl Pts',(1.97603783313957,18.7502583145597,-0.249211496528055));
#24337=CARTESIAN_POINT('Ctrl Pts',(2.07614742951043,18.7760345210385,-0.275621926940948));
#24338=CARTESIAN_POINT('Ctrl Pts',(2.17635351087795,18.7995930649607,-0.304191959203497));
#24339=CARTESIAN_POINT('Ctrl Pts',(2.27056963336781,18.8217433639203,-0.331054177768009));
#24340=CARTESIAN_POINT('Ctrl Pts',(2.36523835232694,18.8419415753925,-0.359935968511773));
#24341=CARTESIAN_POINT('Ctrl Pts',(2.45994739338413,18.8598808531924,-0.390807673438519));
#24342=CARTESIAN_POINT('Ctrl Pts',(2.55421906742605,18.8777372872817,-0.421536812615581));
#24343=CARTESIAN_POINT('Ctrl Pts',(2.64853037015873,18.8933556030678,-0.454237521149386));
#24344=CARTESIAN_POINT('Ctrl Pts',(2.74248535327419,18.9064331858182,-0.488830297490975));
#24345=CARTESIAN_POINT('Ctrl Pts',(2.83620349346067,18.9194778024299,-0.523335871917366));
#24346=CARTESIAN_POINT('Ctrl Pts',(2.92956679712376,18.9299944792857,-0.559723917381846));
#24347=CARTESIAN_POINT('Ctrl Pts',(3.02219766183738,18.9376828843945,-0.597865980324086));
#24348=CARTESIAN_POINT('Ctrl Pts',(3.10530581747092,18.9445809001944,-0.632086933707045));
#24349=CARTESIAN_POINT('Ctrl Pts',(3.18782444335928,18.949202262231,-0.667719091773169));
#24350=CARTESIAN_POINT('Ctrl Pts',(3.26949439648293,18.9513300675967,-0.704636622238322));
#24351=CARTESIAN_POINT('Ctrl Pts',(3.42087322908578,18.9552740479706,-0.773064880742814));
#24352=CARTESIAN_POINT('Ctrl Pts',(3.56980099384823,18.9508507374212,-0.846103860736343));
#24353=CARTESIAN_POINT('Ctrl Pts',(3.71625969440024,18.936539439914,-0.923705011994175));
#24354=CARTESIAN_POINT('Ctrl Pts',(3.74184003411389,18.9340398420711,-0.937258756523275));
#24355=CARTESIAN_POINT('Ctrl Pts',(3.7673450046304,18.9312386033841,-0.950951792714971));
#24356=CARTESIAN_POINT('Ctrl Pts',(3.79277444384618,18.9281276214136,-0.964784010652182));
#24357=CARTESIAN_POINT('Ctrl Pts',(3.86447430656453,18.9193560170413,-1.00378479705462));
#24358=CARTESIAN_POINT('Ctrl Pts',(3.93577353808618,18.9080524652381,-1.04400575073184));
#24359=CARTESIAN_POINT('Ctrl Pts',(4.00627785537283,18.8940495030153,-1.08522709274151));
#24360=CARTESIAN_POINT('Ctrl Pts',(4.07705725420683,18.8799919064571,-1.1266092650518));
#24361=CARTESIAN_POINT('Ctrl Pts',(4.14703529717648,18.8632137942018,-1.16899950567748));
#24362=CARTESIAN_POINT('Ctrl Pts',(4.21584055455503,18.8435457354689,-1.21213051806308));
#24363=CARTESIAN_POINT('Ctrl Pts',(4.24197933063947,18.8360739374869,-1.22851577578894));
#24364=CARTESIAN_POINT('Ctrl Pts',(4.26794914936844,18.828185061729,-1.24500749269148));
#24365=CARTESIAN_POINT('Ctrl Pts',(4.29373077449689,18.8198698188909,-1.26158940397359));
#24366=CARTESIAN_POINT('',(4.29373077449696,18.819869818891,-14.6134105960265));
#24367=CARTESIAN_POINT('Ctrl Pts',(4.29373077449695,18.8198698188909,-1.2615894039735));
#24368=CARTESIAN_POINT('Ctrl Pts',(4.52296127991311,18.7459370341897,-1.40902308532697));
#24369=CARTESIAN_POINT('Ctrl Pts',(4.74196146059745,18.6690215822512,-1.56625194639558));
#24370=CARTESIAN_POINT('Ctrl Pts',(4.95124940534233,18.5902365315365,-1.7332031049152));
#24371=CARTESIAN_POINT('Ctrl Pts',(5.16682135233816,18.5090859100929,-1.90516707703578));
#24372=CARTESIAN_POINT('Ctrl Pts',(5.37208902248157,18.4259511224268,-2.08744583105033));
#24373=CARTESIAN_POINT('Ctrl Pts',(5.56758051817822,18.3420322632787,-2.27999629490369));
#24374=CARTESIAN_POINT('Ctrl Pts',(5.64332797575349,18.3095160650655,-2.35460418533829));
#24375=CARTESIAN_POINT('Ctrl Pts',(5.71760730139922,18.2768820316859,-2.43075460304643));
#24376=CARTESIAN_POINT('Ctrl Pts',(5.79044777763098,18.244199660671,-2.5084465101464));
#24377=CARTESIAN_POINT('Ctrl Pts',(5.79212935934828,18.2434451615186,-2.51024009109646));
#24378=CARTESIAN_POINT('Ctrl Pts',(5.79381016993239,18.242690638533,-2.51203448908584));
#24379=CARTESIAN_POINT('Ctrl Pts',(5.79549020982554,18.2419360925351,-2.51382970417484));
#24380=CARTESIAN_POINT('Ctrl Pts',(5.94895048261904,18.1730134228195,-2.67781045154005));
#24381=CARTESIAN_POINT('Ctrl Pts',(6.0964374109252,18.1036131389842,-2.84947341504703));
#24382=CARTESIAN_POINT('Ctrl Pts',(6.23662479532932,18.0350900643106,-3.02750642175075));
#24383=CARTESIAN_POINT('Ctrl Pts',(6.29721400007292,18.0054742852681,-3.10445256308966));
#24384=CARTESIAN_POINT('Ctrl Pts',(6.3564392068392,17.9760223903775,-3.18258907955983));
#24385=CARTESIAN_POINT('Ctrl Pts',(6.41419086511958,17.9468442552091,-3.26181175077503));
#24386=CARTESIAN_POINT('Ctrl Pts',(6.41654032136261,17.9456572286566,-3.26503469198604));
#24387=CARTESIAN_POINT('Ctrl Pts',(6.41888732415851,17.9444706625731,-3.26825941111731));
#24388=CARTESIAN_POINT('Ctrl Pts',(6.42123186600286,17.9432845644399,-3.27148590089689));
#24389=CARTESIAN_POINT('Ctrl Pts',(6.56679359840251,17.8696452308231,-3.47180369134996));
#24390=CARTESIAN_POINT('Ctrl Pts',(6.70230659932144,17.7981518448203,-3.67790484239893));
#24391=CARTESIAN_POINT('Ctrl Pts',(6.82801702238586,17.7297067508609,-3.89000132125883));
#24392=CARTESIAN_POINT('Ctrl Pts',(6.86647149533936,17.7087695847111,-3.95488105128465));
#24393=CARTESIAN_POINT('Ctrl Pts',(6.90400842024961,17.6881177916226,-4.02032196158267));
#24394=CARTESIAN_POINT('Ctrl Pts',(6.94063408540424,17.6677776026631,-4.08633059633637));
#24395=CARTESIAN_POINT('Ctrl Pts',(6.94307149280366,17.6664239800909,-4.0907234158004));
#24396=CARTESIAN_POINT('Ctrl Pts',(6.94550485844198,17.6650717410359,-4.09511873913086));
#24397=CARTESIAN_POINT('Ctrl Pts',(6.9479341839415,17.6637208933711,-4.09951656782928));
#24398=CARTESIAN_POINT('Ctrl Pts',(7.07457713214333,17.5932999757631,-4.32877937849984));
#24399=CARTESIAN_POINT('Ctrl Pts',(7.19024425834999,17.5266506308987,-4.56484689159181));
#24400=CARTESIAN_POINT('Ctrl Pts',(7.29463565870743,17.4650089179656,-4.8082323477729));
#24401=CARTESIAN_POINT('Ctrl Pts',(7.31828389376895,17.4510449543436,-4.86336750697776));
#24402=CARTESIAN_POINT('Ctrl Pts',(7.3413533442809,17.4373380948032,-4.91887830496527));
#24403=CARTESIAN_POINT('Ctrl Pts',(7.36384027657162,17.4239029374496,-4.97477088449852));
#24404=CARTESIAN_POINT('Ctrl Pts',(7.36582071204235,17.4227196963639,-4.97969337217391));
#24405=CARTESIAN_POINT('Ctrl Pts',(7.3677966465828,17.421538551103,-4.98461886435727));
#24406=CARTESIAN_POINT('Ctrl Pts',(7.36976807627247,17.4203595125087,-4.98954736266744));
#24407=CARTESIAN_POINT('Ctrl Pts',(7.44546738549149,17.3750865780502,-5.17879272075504));
#24408=CARTESIAN_POINT('Ctrl Pts',(7.51472895158381,17.3327859329729,-5.37351256296032));
#24409=CARTESIAN_POINT('Ctrl Pts',(7.57645236778969,17.2945594351273,-5.57103119962675));
#24410=CARTESIAN_POINT('Ctrl Pts',(7.6134892377392,17.2716217897998,-5.68955140651901));
#24411=CARTESIAN_POINT('Ctrl Pts',(7.64781231105249,17.2501510470144,-5.80907812835044));
#24412=CARTESIAN_POINT('Ctrl Pts',(7.67918843644891,17.2303836853409,-5.92902599543444));
#24413=CARTESIAN_POINT('Ctrl Pts',(7.68031341058553,17.2296749371971,-5.93332666183312));
#24414=CARTESIAN_POINT('Ctrl Pts',(7.68143460129584,17.228968374108,-5.93762788663628));
#24415=CARTESIAN_POINT('Ctrl Pts',(7.68255199817302,17.2282640067419,-5.94192964406954));
#24416=CARTESIAN_POINT('Ctrl Pts',(7.79057552101168,17.1601698086902,-6.35779888608028));
#24417=CARTESIAN_POINT('Ctrl Pts',(7.86480882895862,17.1119590389104,-6.7800537358947));
#24418=CARTESIAN_POINT('Ctrl Pts',(7.90422422578528,17.0860934796973,-7.20900733101881));
#24419=CARTESIAN_POINT('Ctrl Pts',(7.92603246422657,17.0717822630624,-7.44634408355374));
#24420=CARTESIAN_POINT('Ctrl Pts',(7.9371813500858,17.0643124088864,-7.68573164451451));
#24421=CARTESIAN_POINT('Ctrl Pts',(7.93749334978002,17.0641067984408,-7.92722383823945));
#24422=CARTESIAN_POINT('Ctrl Pts',(7.93749390429189,17.0641064330128,-7.92765303830522));
#24423=CARTESIAN_POINT('Ctrl Pts',(7.93749442457205,17.0641060905316,-7.92808224486615));
#24424=CARTESIAN_POINT('Ctrl Pts',(7.93749491061955,17.0641057709997,-7.92851145792049));
#24425=CARTESIAN_POINT('Ctrl Pts',(7.93768655372469,17.0639797831163,-8.09774537352705));
#24426=CARTESIAN_POINT('Ctrl Pts',(7.93239900403588,17.0674615298841,-8.26868081960914));
#24427=CARTESIAN_POINT('Ctrl Pts',(7.92171494756793,17.0744688979786,-8.43783842494743));
#24428=CARTESIAN_POINT('Ctrl Pts',(7.91102345406277,17.0814811438138,-8.60711377876527));
#24429=CARTESIAN_POINT('Ctrl Pts',(7.89497393957297,17.0919932010127,-8.77503336987718));
#24430=CARTESIAN_POINT('Ctrl Pts',(7.87374400759939,17.1058076114061,-8.9415226853975));
#24431=CARTESIAN_POINT('Ctrl Pts',(7.87346433385428,17.1059895963459,-8.94371594209044));
#24432=CARTESIAN_POINT('Ctrl Pts',(7.87318376431306,17.1061721542786,-8.94590895118223));
#24433=CARTESIAN_POINT('Ctrl Pts',(7.87290229918002,17.1063552847221,-8.94810171246737));
#24434=CARTESIAN_POINT('Ctrl Pts',(7.83036082814314,17.1340341605142,-9.27952212569055));
#24435=CARTESIAN_POINT('Ctrl Pts',(7.76731445840908,17.1748198120981,-9.60560706040417));
#24436=CARTESIAN_POINT('Ctrl Pts',(7.6842640760672,17.2271865562987,-9.92646753600803));
#24437=CARTESIAN_POINT('Ctrl Pts',(7.68326626852899,17.2278157157395,-9.93032250924526));
#24438=CARTESIAN_POINT('Ctrl Pts',(7.68226543432046,17.2284466292013,-9.93417703697893));
#24439=CARTESIAN_POINT('Ctrl Pts',(7.68126157924107,17.2290792899692,-9.93803110380722));
#24440=CARTESIAN_POINT('Ctrl Pts',(7.6271922995878,17.2631554357069,-10.1456174590694));
#24441=CARTESIAN_POINT('Ctrl Pts',(7.56432398390477,17.3023261323862,-10.3519881859263));
#24442=CARTESIAN_POINT('Ctrl Pts',(7.49357630934712,17.3455332820285,-10.5546437946154));
#24443=CARTESIAN_POINT('Ctrl Pts',(7.45531251783705,17.3689018150015,-10.6642498277141));
#24444=CARTESIAN_POINT('Ctrl Pts',(7.41474450629143,17.3934507919441,-10.7727695920332));
#24445=CARTESIAN_POINT('Ctrl Pts',(7.37202153836162,17.4190115694055,-10.8798128127264));
#24446=CARTESIAN_POINT('Ctrl Pts',(7.37020264317797,17.4200997984605,-10.8843700897133));
#24447=CARTESIAN_POINT('Ctrl Pts',(7.36837989989913,17.4211898298959,-10.8889247935219));
#24448=CARTESIAN_POINT('Ctrl Pts',(7.36655331157689,17.4222816552053,-10.8934769256074));
#24449=CARTESIAN_POINT('Ctrl Pts',(7.26791525731588,17.4812415876656,-11.1392977524395));
#24450=CARTESIAN_POINT('Ctrl Pts',(7.15804389787725,17.5454461271643,-11.3776798579793));
#24451=CARTESIAN_POINT('Ctrl Pts',(7.03725813907874,17.6136630594658,-11.6091505327106));
#24452=CARTESIAN_POINT('Ctrl Pts',(7.00830992726388,17.6300123230318,-11.6646261300634));
#24453=CARTESIAN_POINT('Ctrl Pts',(6.97873464026834,17.6465921970398,-11.7197046258927));
#24454=CARTESIAN_POINT('Ctrl Pts',(6.94853637755767,17.6633859685255,-11.7743930737979));
#24455=CARTESIAN_POINT('Ctrl Pts',(6.94626438275751,17.6646494637754,-11.7785076107983));
#24456=CARTESIAN_POINT('Ctrl Pts',(6.94398886116031,17.6659141722403,-11.7826199391936));
#24457=CARTESIAN_POINT('Ctrl Pts',(6.94170981151122,17.6671800874607,-11.7867300602744));
#24458=CARTESIAN_POINT('Ctrl Pts',(6.81695592061704,17.7364755718065,-12.0117157673991));
#24459=CARTESIAN_POINT('Ctrl Pts',(6.6816450337051,17.8093783830793,-12.2300694172962));
#24460=CARTESIAN_POINT('Ctrl Pts',(6.53553788079947,17.884850092244,-12.4420279462862));
#24461=CARTESIAN_POINT('Ctrl Pts',(6.49757915907396,17.9044576853657,-12.4970948931076));
#24462=CARTESIAN_POINT('Ctrl Pts',(6.45889152050604,17.9242387878342,-12.551730058623));
#24463=CARTESIAN_POINT('Ctrl Pts',(6.41947032548394,17.9441754145465,-12.6059373178004));
#24464=CARTESIAN_POINT('Ctrl Pts',(6.26576753853644,18.0219080932814,-12.8172907991874));
#24465=CARTESIAN_POINT('Ctrl Pts',(6.10302120090262,18.1009132291616,-13.0192031751115));
#24466=CARTESIAN_POINT('Ctrl Pts',(5.93170231123652,18.1799349592224,-13.2118610040649));
#24467=CARTESIAN_POINT('Ctrl Pts',(5.88659280060703,18.2007419559236,-13.2625892127287));
#24468=CARTESIAN_POINT('Ctrl Pts',(5.84088875212914,18.2215501339452,-13.3126755966646));
#24469=CARTESIAN_POINT('Ctrl Pts',(5.79459835582526,18.2423366010449,-13.3621231338839));
#24470=CARTESIAN_POINT('Ctrl Pts',(5.79304324259934,18.2430349167321,-13.3637843103969));
#24471=CARTESIAN_POINT('Ctrl Pts',(5.79148746488082,18.2437332148296,-13.3654447918941));
#24472=CARTESIAN_POINT('Ctrl Pts',(5.78993102234957,18.2444314946609,-13.3671045783627));
#24473=CARTESIAN_POINT('Ctrl Pts',(5.60237021613349,18.3285784679638,-13.5671189585611));
#24474=CARTESIAN_POINT('Ctrl Pts',(5.40518143553207,18.4124500510806,-13.7570185296695));
#24475=CARTESIAN_POINT('Ctrl Pts',(5.19781723993319,18.4948497470905,-13.9367452846217));
#24476=CARTESIAN_POINT('Ctrl Pts',(4.99678320746859,18.5747340449313,-14.1109855587706));
#24477=CARTESIAN_POINT('Ctrl Pts',(4.78618558508331,18.653235544217,-14.2756645218748));
#24478=CARTESIAN_POINT('Ctrl Pts',(4.56549140125338,18.7292531897088,-14.4306961708455));
#24479=CARTESIAN_POINT('Ctrl Pts',(4.47655669712446,18.7598865607069,-14.4931703765203));
#24480=CARTESIAN_POINT('Ctrl Pts',(4.38598200610592,18.7901164034845,-14.5540775737448));
#24481=CARTESIAN_POINT('Ctrl Pts',(4.29373077449694,18.819869818891,-14.6134105960265));
#24482=CARTESIAN_POINT('Ctrl Pts',(4.29373077449694,18.819869818891,-14.6134105960265));
#24483=CARTESIAN_POINT('Ctrl Pts',(4.2258264894115,18.8417707121597,-14.6570844461174));
#24484=CARTESIAN_POINT('Ctrl Pts',(4.15661453194596,18.8607138863202,-14.7001296121417));
#24485=CARTESIAN_POINT('Ctrl Pts',(4.08645576680384,18.876869061117,-14.7422619734974));
#24486=CARTESIAN_POINT('Ctrl Pts',(4.01660140109238,18.8929541430893,-14.7842115342182));
#24487=CARTESIAN_POINT('Ctrl Pts',(3.94580863051476,18.9062753659278,-14.8252560243148));
#24488=CARTESIAN_POINT('Ctrl Pts',(3.87446194432254,18.9170002498469,-14.8651583989106));
#24489=CARTESIAN_POINT('Ctrl Pts',(3.84731136562891,18.9210815438826,-14.8803430223227));
#24490=CARTESIAN_POINT('Ctrl Pts',(3.82008084867992,18.9247868516778,-14.8953627133163));
#24491=CARTESIAN_POINT('Ctrl Pts',(3.79279256087219,18.9281254049619,-14.9102061346505));
#24492=CARTESIAN_POINT('Ctrl Pts',(3.64719779704913,18.9459380240731,-14.9894021779752));
#24493=CARTESIAN_POINT('Ctrl Pts',(3.49912877542333,18.9535969347799,-15.0640395739358));
#24494=CARTESIAN_POINT('Ctrl Pts',(3.34860693025921,18.952622880884,-15.1340782061074));
#24495=CARTESIAN_POINT('Ctrl Pts',(3.32232346104436,18.9524527958339,-15.1463080471018));
#24496=CARTESIAN_POINT('Ctrl Pts',(3.29596515519248,18.9520194863078,-15.158397549995));
#24497=CARTESIAN_POINT('Ctrl Pts',(3.26953206999647,18.9513310489587,-15.1703463479646));
#24498=CARTESIAN_POINT('Ctrl Pts',(3.17850334583779,18.9489602483847,-15.2114949246949));
#24499=CARTESIAN_POINT('Ctrl Pts',(3.08641987565695,18.9434916030852,-15.2510459153296));
#24500=CARTESIAN_POINT('Ctrl Pts',(2.99364161461558,18.9352254582242,-15.2888275082289));
#24501=CARTESIAN_POINT('Ctrl Pts',(2.90078198108108,18.9269520634234,-15.3266422380114));
#24502=CARTESIAN_POINT('Ctrl Pts',(2.80722663233789,18.9158762597357,-15.3626843418299));
#24503=CARTESIAN_POINT('Ctrl Pts',(2.71335601231308,18.9022991832847,-15.3968300905943));
#24504=CARTESIAN_POINT('Ctrl Pts',(2.61888384721251,18.8886351017251,-15.4311946533712));
#24505=CARTESIAN_POINT('Ctrl Pts',(2.52409266754301,18.8724375871946,-15.4636383829821));
#24506=CARTESIAN_POINT('Ctrl Pts',(2.42938551103024,18.8540136022486,-15.4940860207369));
#24507=CARTESIAN_POINT('Ctrl Pts',(2.34490238900942,18.8375785636981,-15.5212467083809));
#24508=CARTESIAN_POINT('Ctrl Pts',(2.26048649576885,18.8193718208331,-15.5468197310283));
#24509=CARTESIAN_POINT('Ctrl Pts',(2.17643094124152,18.7996112684571,-15.5707859639874));
#24510=CARTESIAN_POINT('Ctrl Pts',(2.04502170239011,18.7687183767071,-15.6082538558954));
#24511=CARTESIAN_POINT('Ctrl Pts',(1.91377939287443,18.7340115684464,-15.6420092988788));
#24512=CARTESIAN_POINT('Ctrl Pts',(1.78264791444772,18.6958884625519,-15.672231583133));
#24513=CARTESIAN_POINT('Ctrl Pts',(1.64965288012492,18.6572235756936,-15.7028833669757));
#24514=CARTESIAN_POINT('Ctrl Pts',(1.5167714083236,18.6150446008053,-15.7299010323556));
#24515=CARTESIAN_POINT('Ctrl Pts',(1.38391902822637,18.5697663509256,-15.753424409391));
#24516=CARTESIAN_POINT('Ctrl Pts',(1.28346880481848,18.5355312825542,-15.7712105301724));
#24517=CARTESIAN_POINT('Ctrl Pts',(1.18303463224972,18.4995243793018,-15.7869980223658));
#24518=CARTESIAN_POINT('Ctrl Pts',(1.08257270443595,18.4619249481094,-15.8008289763058));
#24519=CARTESIAN_POINT('Ctrl Pts',(0.977468955166276,18.4225882434021,-15.815298986455));
#24520=CARTESIAN_POINT('Ctrl Pts',(0.872311892509042,18.3814503563707,-15.8276247097051));
#24521=CARTESIAN_POINT('Ctrl Pts',(0.767497582477098,18.3388427147692,-15.8378071909194));
#24522=CARTESIAN_POINT('Ctrl Pts',(0.690645617489172,18.3076019330517,-15.8452731914066));
#24523=CARTESIAN_POINT('Ctrl Pts',(0.613978042671126,18.2755709939336,-15.8515880632921));
#24524=CARTESIAN_POINT('Ctrl Pts',(0.537651063225676,18.2428805421952,-15.8567700158672));
#24525=CARTESIAN_POINT('Ctrl Pts',(0.45595667868505,18.2078912585301,-15.8623163695866));
#24526=CARTESIAN_POINT('Ctrl Pts',(0.374796918314128,18.1722049684796,-15.8665608418546));
#24527=CARTESIAN_POINT('Ctrl Pts',(0.293782657351695,18.135742245179,-15.8695613966509));
#24528=CARTESIAN_POINT('Ctrl Pts',(0.212550494338228,18.0991814489947,-15.8725700219652));
#24529=CARTESIAN_POINT('Ctrl Pts',(0.131464343430913,18.0618400372367,-15.8743280246751));
#24530=CARTESIAN_POINT('Ctrl Pts',(0.0501289083873587,18.0236379404178,
-15.8748417050386));
#24531=CARTESIAN_POINT('Ctrl Pts',(0.0334309211470233,18.0157951333449,
-15.8749471624957));
#24532=CARTESIAN_POINT('Ctrl Pts',(0.0167224250241153,18.0079160508122,
-15.875));
#24533=CARTESIAN_POINT('Ctrl Pts',(4.32715606350417E-14,18.0000000000001,
-15.875));
#24534=CARTESIAN_POINT('',(4.52144207627622,18.7773513853136,-1.41366157655261));
#24535=CARTESIAN_POINT('Ctrl Pts',(1.73472347597681E-15,19.8025000069371,
-15.875));
#24536=CARTESIAN_POINT('Ctrl Pts',(0.28078511621843,19.7879617713667,-15.875));
#24537=CARTESIAN_POINT('Ctrl Pts',(0.561903033215541,19.7734063043411,-15.8601014606599));
#24538=CARTESIAN_POINT('Ctrl Pts',(1.86117102937661,19.7061339914361,-15.7214667453191));
#24539=CARTESIAN_POINT('Ctrl Pts',(2.84950805886979,19.6567506265481,-15.4164312891935));
#24540=CARTESIAN_POINT('Ctrl Pts',(4.6649970185884,19.5510594075386,-14.4424148382232));
#24541=CARTESIAN_POINT('Ctrl Pts',(5.47292612938169,19.497026701168,-13.7790166836516));
#24542=CARTESIAN_POINT('Ctrl Pts',(6.7922170125074,19.39294016586,-12.1747691802672));
#24543=CARTESIAN_POINT('Ctrl Pts',(7.28903180110871,19.340889707494,-11.2479079619773));
#24544=CARTESIAN_POINT('Ctrl Pts',(7.89112344354121,19.2339761464206,-9.27239428384591));
#24545=CARTESIAN_POINT('Ctrl Pts',(7.99733713518596,19.1835834316776,-8.2446715787786));
#24546=CARTESIAN_POINT('Ctrl Pts',(7.81173773313659,19.0791855521311,-6.18491852326425));
#24547=CARTESIAN_POINT('Ctrl Pts',(7.51360210287129,19.0246028887965,-5.17335226229376));
#24548=CARTESIAN_POINT('Ctrl Pts',(6.7337446239372,18.9389600978562,-3.68755396639768));
#24549=CARTESIAN_POINT('Ctrl Pts',(6.37318980270495,18.9081830882073,-3.16384313246412));
#24550=CARTESIAN_POINT('Ctrl Pts',(5.52988896127073,18.8437451698883,-2.20723351035506));
#24551=CARTESIAN_POINT('Ctrl Pts',(5.04878532190664,18.8105640618459,-1.77914455941684));
#24552=CARTESIAN_POINT('Ctrl Pts',(4.52144207733339,18.7773513820815,-1.41366157532098));
#24553=CARTESIAN_POINT('',(4.52144288377396,20.9998514252466,-1.41366213469196));
#24554=CARTESIAN_POINT('',(4.52144227190804,-18.001,-1.41366171017376));
#24555=CARTESIAN_POINT('Ctrl Pts',(4.52144288411286,20.9998514259562,-1.41366213447142));
#24556=CARTESIAN_POINT('Ctrl Pts',(4.5383926725966,21.0009189430859,-1.42540943753239));
#24557=CARTESIAN_POINT('Ctrl Pts',(4.55728556841932,21.0021118120135,-1.43860111654245));
#24558=CARTESIAN_POINT('Ctrl Pts',(4.59656734244123,21.0046012578358,-1.46633308801974));
#24559=CARTESIAN_POINT('Ctrl Pts',(4.61525107330043,21.0057890269683,-1.47964508784235));
#24560=CARTESIAN_POINT('Ctrl Pts',(4.67112900535412,21.0093524693881,-1.51982399655622));
#24561=CARTESIAN_POINT('Ctrl Pts',(4.70814823049889,21.0117281688305,-1.54693259872643));
#24562=CARTESIAN_POINT('Ctrl Pts',(4.81847839168823,21.0188535923946,-1.62920471299908));
#24563=CARTESIAN_POINT('Ctrl Pts',(4.89107015989642,21.0236021542917,-1.68531988610988));
#24564=CARTESIAN_POINT('Ctrl Pts',(5.10566975846148,21.0378234731235,-1.85723573883025));
#24565=CARTESIAN_POINT('Ctrl Pts',(5.24465837470424,21.0472815114198,-1.97670838228095));
#24566=CARTESIAN_POINT('Ctrl Pts',(5.64698140301046,21.0754192752053,-2.34751435539956));
#24567=CARTESIAN_POINT('Ctrl Pts',(5.89730544927446,21.0939623080549,-2.61226344399402));
#24568=CARTESIAN_POINT('Ctrl Pts',(6.58950342094494,21.1485522388563,-3.45326123482118));
#24569=CARTESIAN_POINT('Ctrl Pts',(6.97149805034829,21.1842837666164,-4.07379455621954));
#24570=CARTESIAN_POINT('Ctrl Pts',(7.68790162509451,21.2758275495856,-5.70004455898083));
#24571=CARTESIAN_POINT('Ctrl Pts',(7.9164252601042,21.3305618299046,-6.73730808732291));
#24572=CARTESIAN_POINT('Ctrl Pts',(7.9553382818272,21.4335563885068,-8.81622452353918));
#24573=CARTESIAN_POINT('Ctrl Pts',(7.77492400159749,21.4861693008238,-9.83763210663414));
#24574=CARTESIAN_POINT('Ctrl Pts',(7.03333162878123,21.5926233167573,-11.758487045622));
#24575=CARTESIAN_POINT('Ctrl Pts',(6.47786512863979,21.6427390970134,-12.6390947482521));
#24576=CARTESIAN_POINT('Ctrl Pts',(5.05339855943061,21.7482904710141,-14.1467122935227));
#24577=CARTESIAN_POINT('Ctrl Pts',(4.19490628033729,21.8027988640264,-14.7561464216009));
#24578=CARTESIAN_POINT('Ctrl Pts',(2.30914815337798,21.9074823693995,-15.6003340105396));
#24579=CARTESIAN_POINT('Ctrl Pts',(1.30300839224804,21.9575340202796,-15.8339134177512));
#24580=CARTESIAN_POINT('Ctrl Pts',(0.186818041394457,22.0153271058986,-15.8733523298983));
#24581=CARTESIAN_POINT('Ctrl Pts',(0.0933755231575857,22.0201652873541,
-15.875));
#24582=CARTESIAN_POINT('Ctrl Pts',(-6.13136191901172E-14,22.0250000000001,
-15.875));
#24583=CARTESIAN_POINT('Origin',(0.,-18.001,-7.93750000000004));
#24584=CARTESIAN_POINT('',(-1.46435436667273E-14,24.8825000069372,-15.875));
#24585=CARTESIAN_POINT('',(2.4976926802685E-15,24.565,-15.875));
#24586=CARTESIAN_POINT('',(-9.72063396823211E-16,-18.001,-15.875));
#24587=CARTESIAN_POINT('Ctrl Pts',(5.27355936696949E-15,24.8825000069372,
-15.875));
#24588=CARTESIAN_POINT('Ctrl Pts',(0.508585808332571,24.8561669149667,-15.875));
#24589=CARTESIAN_POINT('Ctrl Pts',(1.0172159760106,24.8298315261982,-15.8261195652966));
#24590=CARTESIAN_POINT('Ctrl Pts',(2.53199346929553,24.7514007591734,-15.5308196961735));
#24591=CARTESIAN_POINT('Ctrl Pts',(3.49697445619331,24.7011416007129,-15.1375440354767));
#24592=CARTESIAN_POINT('Ctrl Pts',(5.21784645322123,24.5946348231499,-14.006500726105));
#24593=CARTESIAN_POINT('Ctrl Pts',(5.9584541853683,24.542304507375,-13.2812058307267));
#24594=CARTESIAN_POINT('Ctrl Pts',(7.13587120049114,24.4391532565869,-11.5690297426178));
#24595=CARTESIAN_POINT('Ctrl Pts',(7.55349651279749,24.3844224072545,-10.593278748503));
#24596=CARTESIAN_POINT('Ctrl Pts',(7.97902505515585,24.2775641934729,-8.56152020560536));
#24597=CARTESIAN_POINT('Ctrl Pts',(7.99286614193217,24.2281815440205,-7.52720113107582));
#24598=CARTESIAN_POINT('Ctrl Pts',(7.6246493370653,24.1224735020145,-5.50017796733907));
#24599=CARTESIAN_POINT('Ctrl Pts',(7.2420712931667,24.0684529590819,-4.52746395914797));
#24600=CARTESIAN_POINT('Ctrl Pts',(6.1215593228575,23.9643987393829,-2.77846127714132));
#24601=CARTESIAN_POINT('Ctrl Pts',(5.39233178046772,23.9122970839216,-2.02040129161139));
#24602=CARTESIAN_POINT('Ctrl Pts',(3.69765257712498,23.8053755570064,-0.839678779680375));
#24603=CARTESIAN_POINT('Ctrl Pts',(2.75247326215505,23.7550150562583,-0.422476472920795));
#24604=CARTESIAN_POINT('Ctrl Pts',(0.735688572314485,23.6505918186215,0.0345284891707951));
#24605=CARTESIAN_POINT('Ctrl Pts',(-0.318384469253613,23.5960149863692,
0.0620656974416982));
#24606=CARTESIAN_POINT('Ctrl Pts',(-2.36232482748936,23.49018570731,-0.290032971156351));
#24607=CARTESIAN_POINT('Ctrl Pts',(-3.33346000867118,23.4403280501711,-0.660664150701976));
#24608=CARTESIAN_POINT('Ctrl Pts',(-5.07935293483514,23.3339880940002,-1.75178765582861));
#24609=CARTESIAN_POINT('Ctrl Pts',(-5.8375698374364,23.2807466706889,-2.46163280366343));
#24610=CARTESIAN_POINT('Ctrl Pts',(-7.05508863841836,23.1780879761606,-4.1507764548021));
#24611=CARTESIAN_POINT('Ctrl Pts',(-7.49477280115995,23.1233551647315,-5.11939993917488));
#24612=CARTESIAN_POINT('Ctrl Pts',(-7.96374159160696,23.0162032347313,-7.14300852639246));
#24613=CARTESIAN_POINT('Ctrl Pts',(-7.99972513178049,22.9667573095989,-8.175875293155));
#24614=CARTESIAN_POINT('Ctrl Pts',(-7.67519193208713,22.8613172543984,-10.2116499836502));
#24615=CARTESIAN_POINT('Ctrl Pts',(-7.31254814444144,22.8071240726913,-11.1943468829651));
#24616=CARTESIAN_POINT('Ctrl Pts',(-6.22935447415169,22.7025945863368,-12.9651264842601));
#24617=CARTESIAN_POINT('Ctrl Pts',(-5.5190149938795,22.6512135864572,-13.7359830183141));
#24618=CARTESIAN_POINT('Ctrl Pts',(-3.85314485337722,22.5444176707724,-14.9522304452467));
#24619=CARTESIAN_POINT('Ctrl Pts',(-2.91670240612869,22.4935183630391,-15.3904147002793));
#24620=CARTESIAN_POINT('Ctrl Pts',(-1.29256784029279,22.4094254052846,-15.7959532941412));
#24621=CARTESIAN_POINT('Ctrl Pts',(-0.646739751238422,22.3759863077173,
-15.875));
#24622=CARTESIAN_POINT('Ctrl Pts',(5.96744875736022E-14,22.3425000069372,
-15.875));
#24623=CARTESIAN_POINT('Ctrl Pts',(-6.36990460378684E-14,22.0250000000001,
-15.875));
#24624=CARTESIAN_POINT('Ctrl Pts',(-0.949477891510335,22.074161200001,-15.875));
#24625=CARTESIAN_POINT('Ctrl Pts',(-1.89208534878509,22.1218736784768,-15.7046193009312));
#24626=CARTESIAN_POINT('Ctrl Pts',(-3.75092248326721,22.22091379634,-15.0088096691342));
#24627=CARTESIAN_POINT('Ctrl Pts',(-4.63908363095019,22.2747999246053,-14.4606577314775));
#24628=CARTESIAN_POINT('Ctrl Pts',(-6.14924084972979,22.380677195981,-13.060274847696));
#24629=CARTESIAN_POINT('Ctrl Pts',(-6.75905812878465,22.4300820990418,-12.2236544338043));
#24630=CARTESIAN_POINT('Ctrl Pts',(-7.63659592255119,22.5367202762854,-10.343230987385));
#24631=CARTESIAN_POINT('Ctrl Pts',(-7.88743301566424,22.5914348158204,-9.31361842665414));
#24632=CARTESIAN_POINT('Ctrl Pts',(-7.97306761740581,22.6949093830429,-7.24013498608011));
#24633=CARTESIAN_POINT('Ctrl Pts',(-7.8163219568117,22.7466803925623,-6.21661270669918));
#24634=CARTESIAN_POINT('Ctrl Pts',(-7.11913434193015,22.8532950466548,-4.27806763088598));
#24635=CARTESIAN_POINT('Ctrl Pts',(-6.58228163977797,22.9039007232003,-3.38260125949016));
#24636=CARTESIAN_POINT('Ctrl Pts',(-5.19122591377799,23.0090123617593,-1.84344654635718));
#24637=CARTESIAN_POINT('Ctrl Pts',(-4.34864002346912,23.0633959832718,-1.21621891854341));
#24638=CARTESIAN_POINT('Ctrl Pts',(-2.48493043657753,23.1684396065758,-0.32985129266046));
#24639=CARTESIAN_POINT('Ctrl Pts',(-1.48444474350808,23.2181397744191,-0.0731761849580272));
#24640=CARTESIAN_POINT('Ctrl Pts',(0.584239367992702,23.3252502129597,0.0476526856448932));
#24641=CARTESIAN_POINT('Ctrl Pts',(1.63304041198226,23.3788605119783,-0.0993363107181023));
#24642=CARTESIAN_POINT('Ctrl Pts',(3.59655181222106,23.4820300205898,-0.786758499983969));
#24643=CARTESIAN_POINT('Ctrl Pts',(4.49450140548816,23.5356971537053,-1.31424201288508));
#24644=CARTESIAN_POINT('Ctrl Pts',(6.0349478213324,23.641797199696,-2.68025536507279));
#24645=CARTESIAN_POINT('Ctrl Pts',(6.6639671087408,23.6913334759273,-3.50458001374237));
#24646=CARTESIAN_POINT('Ctrl Pts',(7.58169225846245,23.7976250644636,-5.36490745307786));
#24647=CARTESIAN_POINT('Ctrl Pts',(7.85458790513208,23.8522936097784,-6.38641872853286));
#24648=CARTESIAN_POINT('Ctrl Pts',(7.98667256090725,23.9562149288905,-8.45388203717645));
#24649=CARTESIAN_POINT('Ctrl Pts',(7.85341991252846,24.007273438891,-9.47940961671702));
#24650=CARTESIAN_POINT('Ctrl Pts',(7.20039415369292,24.114034653206,-11.4352800183161));
#24651=CARTESIAN_POINT('Ctrl Pts',(6.68210414203887,24.1652456157174,-12.3454014227126));
#24652=CARTESIAN_POINT('Ctrl Pts',(5.32434865180305,24.269894965243,-13.9151999953278));
#24653=CARTESIAN_POINT('Ctrl Pts',(4.4977673852279,24.3241294065212,-14.5595543047395));
#24654=CARTESIAN_POINT('Ctrl Pts',(2.6562899853584,24.4294944312366,-15.4870825809801));
#24655=CARTESIAN_POINT('Ctrl Pts',(1.66143917596496,24.4789755181781,-15.7663991960582));
#24656=CARTESIAN_POINT('Ctrl Pts',(0.427422115449422,24.5428693276696,-15.8663795220757));
#24657=CARTESIAN_POINT('Ctrl Pts',(0.21358319137833,24.5539412843816,-15.875));
#24658=CARTESIAN_POINT('Ctrl Pts',(-4.76702011198427E-14,24.565,-15.875));
#24659=CARTESIAN_POINT('Origin',(0.,-18.001,-7.93750000000004));
#24660=CARTESIAN_POINT('',(7.49369629108171E-15,27.4225000069372,-15.875));
#24661=CARTESIAN_POINT('',(-5.16978508354899E-15,27.1050000000001,-15.875));
#24662=CARTESIAN_POINT('',(-9.72063396823211E-16,-18.001,-15.875));
#24663=CARTESIAN_POINT('Ctrl Pts',(9.5062846483529E-14,27.4225000069372,
-15.875));
#24664=CARTESIAN_POINT('Ctrl Pts',(0.624219539852169,27.3901797371156,-15.875));
#24665=CARTESIAN_POINT('Ctrl Pts',(1.24771112812793,27.3578971585064,-15.801362942656));
#24666=CARTESIAN_POINT('Ctrl Pts',(2.86701695199915,27.2740542189479,-15.4116256134532));
#24667=CARTESIAN_POINT('Ctrl Pts',(3.81924123505487,27.2226292642049,-14.9728242497032));
#24668=CARTESIAN_POINT('Ctrl Pts',(5.48912016231564,27.1158247420042,-13.7618116498142));
#24669=CARTESIAN_POINT('Ctrl Pts',(6.19410644258195,27.064964283629,-13.0056376260485));
#24670=CARTESIAN_POINT('Ctrl Pts',(7.28947994752642,26.9609089493055,-11.2484443263014));
#24671=CARTESIAN_POINT('Ctrl Pts',(7.6619928698852,26.9062603168654,-10.2597050461275));
#24672=CARTESIAN_POINT('Ctrl Pts',(7.99903184162878,26.800083823255,-8.21303851826056));
#24673=CARTESIAN_POINT('Ctrl Pts',(7.96746790208441,26.7504816783959,-7.17601383432028));
#24674=CARTESIAN_POINT('Ctrl Pts',(7.51002828234806,26.644317832783,-5.16872469739288));
#24675=CARTESIAN_POINT('Ctrl Pts',(7.08732731533967,26.5907251275606,-4.21773572336723));
#24676=CARTESIAN_POINT('Ctrl Pts',(5.89088422543125,26.487731585604,-2.51494425079395));
#24677=CARTESIAN_POINT('Ctrl Pts',(5.12254957469675,26.4337992857223,-1.78392039090943));
#24678=CARTESIAN_POINT('Ctrl Pts',(3.36848207149392,26.326657480458,-0.677700912351653));
#24679=CARTESIAN_POINT('Ctrl Pts',(2.40535199885269,26.2770421281866,-0.304304727598297));
#24680=CARTESIAN_POINT('Ctrl Pts',(0.374502057938519,26.1718906328122,0.0590295397115103));
#24681=CARTESIAN_POINT('Ctrl Pts',(-0.67495984682772,26.1175525517943,0.0392916743172318));
#24682=CARTESIAN_POINT('Ctrl Pts',(-2.70220537666353,26.0125876823283,-0.402670233429265));
#24683=CARTESIAN_POINT('Ctrl Pts',(-3.66081284174792,25.9617990422184,-0.818931376977721));
#24684=CARTESIAN_POINT('Ctrl Pts',(-5.35605729947494,25.8551355586809,-1.99039704350108));
#24685=CARTESIAN_POINT('Ctrl Pts',(-6.07871747524366,25.8036085570719,-2.73131110334026));
#24686=CARTESIAN_POINT('Ctrl Pts',(-7.21494557234268,25.6999861967515,-4.46643733006872));
#24687=CARTESIAN_POINT('Ctrl Pts',(-7.6099153643053,25.6452836412246,-5.44897497305318));
#24688=CARTESIAN_POINT('Ctrl Pts',(-7.99095461069713,25.5387542472933,-7.48851146161607));
#24689=CARTESIAN_POINT('Ctrl Pts',(-7.98202232718952,25.4893198157644,-8.52423487824865));
#24690=CARTESIAN_POINT('Ctrl Pts',(-7.56898602067955,25.3833672804673,-10.5416603459946));
#24691=CARTESIAN_POINT('Ctrl Pts',(-7.16614950446568,25.3295490005744,-11.5036845246756));
#24692=CARTESIAN_POINT('Ctrl Pts',(-6.00744541886707,25.2260123198636,-13.2297679230054));
#24693=CARTESIAN_POINT('Ctrl Pts',(-5.25866306136744,25.1730517413319,-13.9744047651811));
#24694=CARTESIAN_POINT('Ctrl Pts',(-3.53424516529992,25.0660131501615,-15.1180419981786));
#24695=CARTESIAN_POINT('Ctrl Pts',(-2.58006791475045,25.0160884094762,-15.5134055519264));
#24696=CARTESIAN_POINT('Ctrl Pts',(-1.05678757155941,24.9372173896464,-15.8222328513334));
#24697=CARTESIAN_POINT('Ctrl Pts',(-0.528417728937034,24.9098599379989,
-15.875));
#24698=CARTESIAN_POINT('Ctrl Pts',(8.18789480661053E-15,24.8825000069372,
-15.875));
#24699=CARTESIAN_POINT('Ctrl Pts',(-1.17961196366423E-14,24.565,-15.875));
#24700=CARTESIAN_POINT('Ctrl Pts',(-0.836467978306689,24.6083098758209,
-15.875));
#24701=CARTESIAN_POINT('Ctrl Pts',(-1.66901604868968,24.6513687341673,-15.7427642526738));
#24702=CARTESIAN_POINT('Ctrl Pts',(-3.44503997400206,24.7434340320891,-15.162152007294));
#24703=CARTESIAN_POINT('Ctrl Pts',(-4.35204519100589,24.796865006184,-14.6548922502149));
#24704=CARTESIAN_POINT('Ctrl Pts',(-5.92144264644372,24.9031505594052,-13.3226311528391));
#24705=CARTESIAN_POINT('Ctrl Pts',(-6.56905306265197,24.952925693415,-12.5103214269728));
#24706=CARTESIAN_POINT('Ctrl Pts',(-7.52528735905546,25.0588559665969,-10.6698437725775));
#24707=CARTESIAN_POINT('Ctrl Pts',(-7.81923854442363,25.1134553691784,-9.65657797110715));
#24708=CARTESIAN_POINT('Ctrl Pts',(-7.99593679652942,25.2177768367742,-7.59548449089693));
#24709=CARTESIAN_POINT('Ctrl Pts',(-7.88522677580753,25.2682687366265,-6.56811852720181));
#24710=CARTESIAN_POINT('Ctrl Pts',(-7.27465739000588,25.3751581999211,-4.59584880005299));
#24711=CARTESIAN_POINT('Ctrl Pts',(-6.77426313425,25.4270586590243,-3.67176122202902));
#24712=CARTESIAN_POINT('Ctrl Pts',(-5.44856714317156,25.5312410147699,-2.07318110685299));
#24713=CARTESIAN_POINT('Ctrl Pts',(-4.63752074881183,25.5853094391607,-1.41289989536927));
#24714=CARTESIAN_POINT('Ctrl Pts',(-2.81768173593427,25.6909496227162,-0.446547711794352));
#24715=CARTESIAN_POINT('Ctrl Pts',(-1.82825937663462,25.7403380540275,-0.1457641783938));
#24716=CARTESIAN_POINT('Ctrl Pts',(0.237099502352091,25.8472763217129,0.065844563319637));
#24717=CARTESIAN_POINT('Ctrl Pts',(1.29420484576369,25.9020101577234,-0.0359189862404865));
#24718=CARTESIAN_POINT('Ctrl Pts',(3.28397585660572,26.0050347057353,-0.638538942803915));
#24719=CARTESIAN_POINT('Ctrl Pts',(4.2002099962157,26.0575929837782,-1.12442905110605));
#24720=CARTESIAN_POINT('Ctrl Pts',(5.79974737504025,26.1640571208062,-2.42107404430918));
#24721=CARTESIAN_POINT('Ctrl Pts',(6.46681553222913,26.2141991661854,-3.22068377432052));
#24722=CARTESIAN_POINT('Ctrl Pts',(7.46292553316076,26.319724597504,-5.03998370845816));
#24723=CARTESIAN_POINT('Ctrl Pts',(7.77858166455462,26.3742261613421,-6.0442102870369));
#24724=CARTESIAN_POINT('Ctrl Pts',(8.00158613360409,26.4789325838569,-8.09807543001832));
#24725=CARTESIAN_POINT('Ctrl Pts',(7.91426666814584,26.5289590715126,-9.12726125824446));
#24726=CARTESIAN_POINT('Ctrl Pts',(7.34783370140172,26.6359683838815,-11.1163056100658));
#24727=CARTESIAN_POINT('Ctrl Pts',(6.86609704238139,26.6886935677963,-12.0547755141607));
#24728=CARTESIAN_POINT('Ctrl Pts',(5.57375337988629,26.792367957767,-13.6825703331671));
#24729=CARTESIAN_POINT('Ctrl Pts',(4.77898461373321,26.8462413617665,-14.3588477598749));
#24730=CARTESIAN_POINT('Ctrl Pts',(2.98189317687904,26.9521332238845,-15.3647789989823));
#24731=CARTESIAN_POINT('Ctrl Pts',(1.99812686687186,27.0015428100985,-15.6875743213914));
#24732=CARTESIAN_POINT('Ctrl Pts',(0.654344113010902,27.0711199675143,-15.8547946639326));
#24733=CARTESIAN_POINT('Ctrl Pts',(0.326990712642387,27.0880693732141,-15.875));
#24734=CARTESIAN_POINT('Ctrl Pts',(-5.25968157916168E-14,27.1050000000001,
-15.875));
#24735=CARTESIAN_POINT('Origin',(0.,-18.001,-7.93750000000004));
#24736=CARTESIAN_POINT('',(-1.32535964816009E-14,29.9625000069372,-15.875));
#24737=CARTESIAN_POINT('',(-4.26571593994078E-14,29.645,-15.875));
#24738=CARTESIAN_POINT('',(-9.72063396823211E-16,-18.001,-15.875));
#24739=CARTESIAN_POINT('Ctrl Pts',(-4.48252546192407E-14,29.9625000069372,
-15.875));
#24740=CARTESIAN_POINT('Ctrl Pts',(0.736573960655214,29.924362352423,-15.875));
#24741=CARTESIAN_POINT('Ctrl Pts',(1.47105355996765,29.8863331378396,-15.772465740066));
#24742=CARTESIAN_POINT('Ctrl Pts',(3.18774470741065,29.7974478698477,-15.2816389743965));
#24743=CARTESIAN_POINT('Ctrl Pts',(4.12686094412051,29.7444249917232,-14.7980669295615));
#24744=CARTESIAN_POINT('Ctrl Pts',(5.74561976414415,29.6373789620042,-13.5087580372874));
#24745=CARTESIAN_POINT('Ctrl Pts',(6.41526615853753,29.5874791981015,-12.7224187313828));
#24746=CARTESIAN_POINT('Ctrl Pts',(7.42815971898147,29.4826519431958,-10.9227503105544));
#24747=CARTESIAN_POINT('Ctrl Pts',(7.75543374230582,29.4281887458617,-9.92307774094497));
#24748=CARTESIAN_POINT('Ctrl Pts',(8.00402649279823,29.3228044342571,-7.86376051477762));
#24749=CARTESIAN_POINT('Ctrl Pts',(7.92659261093737,29.2725134828056,-6.82440623067985));
#24750=CARTESIAN_POINT('Ctrl Pts',(7.37956520218366,29.1659957601636,-4.83903957989797));
#24751=CARTESIAN_POINT('Ctrl Pts',(6.91725543998198,29.1137233616627,-3.91137218888092));
#24752=CARTESIAN_POINT('Ctrl Pts',(5.65038778333555,29.0105394930011,-2.26463030061079));
#24753=CARTESIAN_POINT('Ctrl Pts',(4.85053034642538,28.9558097104299,-1.56721777465549));
#24754=CARTESIAN_POINT('Ctrl Pts',(3.04827483309507,28.8489726456425,-0.537336623884139));
#24755=CARTESIAN_POINT('Ctrl Pts',(2.06829346615786,28.7995902189997,-0.205969067278297));
#24756=CARTESIAN_POINT('Ctrl Pts',(0.0263597995014314,28.6938648405862,
0.0671743779869568));
#24757=CARTESIAN_POINT('Ctrl Pts',(-1.01672316573496,28.6398570424794,0.0023935713156336));
#24758=CARTESIAN_POINT('Ctrl Pts',(-3.02573001584092,28.5358365187321,-0.525708220472481));
#24759=CARTESIAN_POINT('Ctrl Pts',(-3.97158882065666,28.4836811578961,-0.986505905423148));
#24760=CARTESIAN_POINT('Ctrl Pts',(-5.61647909717162,28.3767514102684,-2.23602711384972));
#24761=CARTESIAN_POINT('Ctrl Pts',(-6.3041434221088,28.3264238453969,-3.00704397924283));
#24762=CARTESIAN_POINT('Ctrl Pts',(-7.35921305036772,28.2219743844626,-4.7853365210284));
#24763=CARTESIAN_POINT('Ctrl Pts',(-7.70959913301805,28.1674037307671,-5.77968169536413));
#24764=CARTESIAN_POINT('Ctrl Pts',(-8.003354843952,28.0616011386154,-7.83281881041147));
#24765=CARTESIAN_POINT('Ctrl Pts',(-7.94941043789711,28.0117206267662,-8.87103382953876));
#24766=CARTESIAN_POINT('Ctrl Pts',(-7.44817485664906,27.9053692493889,-10.8679010937008));
#24767=CARTESIAN_POINT('Ctrl Pts',(-7.00603971353237,27.8521917627398,-11.8075725102872));
#24768=CARTESIAN_POINT('Ctrl Pts',(-5.77352473680867,27.74949960399,-13.4854401062041));
#24769=CARTESIAN_POINT('Ctrl Pts',(-4.9872689275275,27.6947661372597,-14.2016947213343));
#24770=CARTESIAN_POINT('Ctrl Pts',(-3.20621013981998,27.5876327327036,-15.2704878517884));
#24771=CARTESIAN_POINT('Ctrl Pts',(-2.23447144379235,27.5381944307113,-15.6225282357278));
#24772=CARTESIAN_POINT('Ctrl Pts',(-0.817251851957353,27.4648149276997,
-15.8434703725885));
#24773=CARTESIAN_POINT('Ctrl Pts',(-0.408470071868316,27.4436493976466,
-15.875));
#24774=CARTESIAN_POINT('Ctrl Pts',(7.08461067588928E-14,27.4225000069372,
-15.875));
#24775=CARTESIAN_POINT('Ctrl Pts',(-5.10702591327572E-14,27.1050000000001,
-15.875));
#24776=CARTESIAN_POINT('Ctrl Pts',(-0.717914112981769,27.1421715019459,
-15.875));
#24777=CARTESIAN_POINT('Ctrl Pts',(-1.43407996200344,27.1792524838758,-15.7775953996811));
#24778=CARTESIAN_POINT('Ctrl Pts',(-3.11674440141664,27.2663759480241,-15.309192321087));
#24779=CARTESIAN_POINT('Ctrl Pts',(-4.0423031180092,27.3180994138876,-14.8451723426533));
#24780=CARTESIAN_POINT('Ctrl Pts',(-5.67239094602482,27.4247234872727,-13.58532121545));
#24781=CARTESIAN_POINT('Ctrl Pts',(-6.35934945246318,27.47536311323,-12.7988363573248));
#24782=CARTESIAN_POINT('Ctrl Pts',(-7.39576329636799,27.5804469591558,-11.0015994225818));
#24783=CARTESIAN_POINT('Ctrl Pts',(-7.73324216548751,27.6348220956183,-10.0070309028449));
#24784=CARTESIAN_POINT('Ctrl Pts',(-8.00316616355678,27.7398865875611,-7.96113935087222));
#24785=CARTESIAN_POINT('Ctrl Pts',(-7.93955543190281,27.7895695346163,-6.93019976657644));
#24786=CARTESIAN_POINT('Ctrl Pts',(-7.41794390221256,27.8966860832206,-4.92441434922844));
#24787=CARTESIAN_POINT('Ctrl Pts',(-6.95521173491136,27.9503570671105,-3.97149099523772));
#24788=CARTESIAN_POINT('Ctrl Pts',(-5.69674018400867,28.0534931347906,-2.31476351275529));
#24789=CARTESIAN_POINT('Ctrl Pts',(-4.91860850865424,28.1071462184412,-1.62282642394335));
#24790=CARTESIAN_POINT('Ctrl Pts',(-3.14485764138248,28.213258720227,-0.577519825724921));
#24791=CARTESIAN_POINT('Ctrl Pts',(-2.16685228936275,28.262806699111,-0.232682623541554));
#24792=CARTESIAN_POINT('Ctrl Pts',(-0.114404512256726,28.3690764675427,
0.067930054342613));
#24793=CARTESIAN_POINT('Ctrl Pts',(0.94137007018476,28.4237414006258,0.0132189985048882));
#24794=CARTESIAN_POINT('Ctrl Pts',(2.94896136887821,28.5276886312436,-0.497265377597983));
#24795=CARTESIAN_POINT('Ctrl Pts',(3.88366732438073,28.5787082396742,-0.93959406668474));
#24796=CARTESIAN_POINT('Ctrl Pts',(5.54382016817213,28.6854778532263,-2.16284643685243));
#24797=CARTESIAN_POINT('Ctrl Pts',(6.25041788147492,28.7367289402747,-2.93621935226714));
#24798=CARTESIAN_POINT('Ctrl Pts',(7.32616862873122,28.8413496814412,-4.71127046121473));
#24799=CARTESIAN_POINT('Ctrl Pts',(7.68482120007732,28.8955743650117,-5.69590390880756));
#24800=CARTESIAN_POINT('Ctrl Pts',(8.00065474910145,29.0009575889456,-7.73335118728829));
#24801=CARTESIAN_POINT('Ctrl Pts',(7.96026661063342,29.0504295279356,-8.76591919118594));
#24802=CARTESIAN_POINT('Ctrl Pts',(7.48263755651254,29.1576366540103,-10.787834781398));
#24803=CARTESIAN_POINT('Ctrl Pts',(7.03861107572573,29.2123372659245,-11.7547821623659));
#24804=CARTESIAN_POINT('Ctrl Pts',(5.81335784329496,29.314924048782,-13.4391822302741));
#24805=CARTESIAN_POINT('Ctrl Pts',(5.05163085685929,29.3683402581132,-14.1459151738609));
#24806=CARTESIAN_POINT('Ctrl Pts',(3.30099691448562,29.4746358794488,-15.2290564673484));
#24807=CARTESIAN_POINT('Ctrl Pts',(2.32866255484483,29.5244286348141,-15.5952242616502));
#24808=CARTESIAN_POINT('Ctrl Pts',(0.87846121798129,29.5995158365285,-15.838565031241));
#24809=CARTESIAN_POINT('Ctrl Pts',(0.439095759214256,29.6222649003928,-15.875));
#24810=CARTESIAN_POINT('Ctrl Pts',(-3.99680288865056E-14,29.645,-15.875));
#24811=CARTESIAN_POINT('Origin',(0.,-18.001,-7.93750000000004));
#24812=CARTESIAN_POINT('',(3.05280419258108E-15,32.5025000069372,-15.875));
#24813=CARTESIAN_POINT('',(2.84491558808815E-14,32.1850000000001,-15.875));
#24814=CARTESIAN_POINT('',(-9.72063396823211E-16,-18.001,-15.875));
#24815=CARTESIAN_POINT('Ctrl Pts',(-1.01307850997046E-14,32.5025000069372,
-15.875));
#24816=CARTESIAN_POINT('Ctrl Pts',(0.849805888356549,32.4584995329788,-15.875));
#24817=CARTESIAN_POINT('Ctrl Pts',(1.69524300201692,32.414903306185,-15.7385137921434));
#24818=CARTESIAN_POINT('Ctrl Pts',(3.50299454566702,32.3208921513219,-15.137633521164));
#24819=CARTESIAN_POINT('Ctrl Pts',(4.42623973950424,32.2661581245547,-14.6099102164331));
#24820=CARTESIAN_POINT('Ctrl Pts',(5.99104322325474,32.1590439672215,-13.2440996243987));
#24821=CARTESIAN_POINT('Ctrl Pts',(6.6249795417268,32.1096130241932,-12.4277417526968));
#24822=CARTESIAN_POINT('Ctrl Pts',(7.55362584166265,32.0041354131546,-10.5874926427543));
#24823=CARTESIAN_POINT('Ctrl Pts',(7.83491766257849,31.9499639421575,-9.57880377695661));
#24824=CARTESIAN_POINT('Ctrl Pts',(7.99369332499519,31.8454964233445,-7.50892096202494));
#24825=CARTESIAN_POINT('Ctrl Pts',(7.86907943675707,31.7940255725315,-6.46765050687525));
#24826=CARTESIAN_POINT('Ctrl Pts',(7.23036751456396,31.6872122133539,-4.5060703270135));
#24827=CARTESIAN_POINT('Ctrl Pts',(6.72774208091398,31.6363913721743,-3.60271706817703));
#24828=CARTESIAN_POINT('Ctrl Pts',(5.39283838888249,31.5323085621847,-2.02008115994509));
#24829=CARTESIAN_POINT('Ctrl Pts',(4.56677207757762,31.4776643982301,-1.36155532801674));
#24830=CARTESIAN_POINT('Ctrl Pts',(2.72309872699471,31.3715122044493,-0.411184564370692));
#24831=CARTESIAN_POINT('Ctrl Pts',(1.72653338920418,31.3218948775435,-0.122146758303137));
#24832=CARTESIAN_POINT('Ctrl Pts',(-0.324117470713751,31.2157181482505,
0.0600801418958527));
#24833=CARTESIAN_POINT('Ctrl Pts',(-1.35887810786185,31.1621412560545,-0.0495340621609275));
#24834=CARTESIAN_POINT('Ctrl Pts',(-3.34733525420087,31.0591847361201,-0.664081986129089));
#24835=CARTESIAN_POINT('Ctrl Pts',(-4.27954278064386,31.0051838630904,-1.17043135315008));
#24836=CARTESIAN_POINT('Ctrl Pts',(-5.87188660873315,30.8980357025591,-2.49945319684862));
#24837=CARTESIAN_POINT('Ctrl Pts',(-6.52342049862927,30.8484363956693,-3.30107633199719));
#24838=CARTESIAN_POINT('Ctrl Pts',(-7.49368309383774,30.7432628065576,-5.12162956841538));
#24839=CARTESIAN_POINT('Ctrl Pts',(-7.79765378547948,30.6889345839556,-6.12613285266895));
#24840=CARTESIAN_POINT('Ctrl Pts',(-8.00073138203963,30.5840007572664,-8.19109063495698));
#24841=CARTESIAN_POINT('Ctrl Pts',(-7.89947037271715,30.5331722793238,-9.23147753227341));
#24842=CARTESIAN_POINT('Ctrl Pts',(-7.30609195072424,30.4264987511991,-11.2049478427975));
#24843=CARTESIAN_POINT('Ctrl Pts',(-6.82338854754,30.3750211664139,-12.1203695415557));
#24844=CARTESIAN_POINT('Ctrl Pts',(-5.52199240182528,30.2713682810967,-13.7349980822292));
#24845=CARTESIAN_POINT('Ctrl Pts',(-4.70870678348807,30.2166685819792,-14.4129398140733));
#24846=CARTESIAN_POINT('Ctrl Pts',(-2.8853352338182,30.1101623486631,-15.4028867093612));
#24847=CARTESIAN_POINT('Ctrl Pts',(-1.8969813878097,30.0607201785052,-15.7130135095793));
#24848=CARTESIAN_POINT('Ctrl Pts',(-0.585223021794811,29.9928011506256,
-15.8588382366372));
#24849=CARTESIAN_POINT('Ctrl Pts',(-0.292446435800955,29.9776420316737,
-15.875));
#24850=CARTESIAN_POINT('Ctrl Pts',(-5.87030424270552E-14,29.9625000069372,
-15.875));
#24851=CARTESIAN_POINT('Ctrl Pts',(-4.53803661315533E-14,29.645,-15.875));
#24852=CARTESIAN_POINT('Ctrl Pts',(-0.60076652805944,29.6761059411745,-15.875));
#24853=CARTESIAN_POINT('Ctrl Pts',(-1.20102819352252,29.7071857420343,-15.8067928930804));
#24854=CARTESIAN_POINT('Ctrl Pts',(-2.78647271976851,29.7892754422182,-15.4399982407669));
#24855=CARTESIAN_POINT('Ctrl Pts',(-3.72985706541699,29.8397374734669,-15.0184674546151));
#24856=CARTESIAN_POINT('Ctrl Pts',(-5.4186118431039,29.946634128663,-13.8304079101059));
#24857=CARTESIAN_POINT('Ctrl Pts',(-6.14395063807967,29.998578603021,-13.0697001623927));
#24858=CARTESIAN_POINT('Ctrl Pts',(-7.25681384791781,30.1027326597859,-11.3161848081354));
#24859=CARTESIAN_POINT('Ctrl Pts',(-7.63531699691702,30.1567905903446,-10.3413875378226));
#24860=CARTESIAN_POINT('Ctrl Pts',(-7.99457161687568,30.2624460277761,-8.31252065008465));
#24861=CARTESIAN_POINT('Ctrl Pts',(-7.97618389438668,30.31183249889,-7.27849297393089));
#24862=CARTESIAN_POINT('Ctrl Pts',(-7.54174953490999,30.4187531380881,-5.24836040346573));
#24863=CARTESIAN_POINT('Ctrl Pts',(-7.11959642041862,30.4734864628244,-4.2740303122445));
#24864=CARTESIAN_POINT('Ctrl Pts',(-5.93394869755091,30.576539362472,-2.56652580710964));
#24865=CARTESIAN_POINT('Ctrl Pts',(-5.18973799987701,30.6290462253603,-1.84438178734286));
#24866=CARTESIAN_POINT('Ctrl Pts',(-3.46373674247435,30.7355199208385,-0.721485316793999));
#24867=CARTESIAN_POINT('Ctrl Pts',(-2.49748880602533,30.7856873032105,-0.332835461595449));
#24868=CARTESIAN_POINT('Ctrl Pts',(-0.459893950304063,30.8911880306299,
0.0549386168117478));
#24869=CARTESIAN_POINT('Ctrl Pts',(0.592598519303625,30.9456830254692,0.0461972746405091));
#24870=CARTESIAN_POINT('Ctrl Pts',(2.61526999568577,31.0504110637688,-0.373671127574245));
#24871=CARTESIAN_POINT('Ctrl Pts',(3.56762371680106,31.1004141393016,-0.773479665864678));
#24872=CARTESIAN_POINT('Ctrl Pts',(5.28600956243452,31.2074300555214,-1.92467424608267));
#24873=CARTESIAN_POINT('Ctrl Pts',(6.03082090822791,31.2602070115457,-2.67205198013382));
#24874=CARTESIAN_POINT('Ctrl Pts',(7.18180568473254,31.363850874488,-4.40282013516036));
#24875=CARTESIAN_POINT('Ctrl Pts',(7.58055982035965,31.4177121364128,-5.36704361649729));
#24876=CARTESIAN_POINT('Ctrl Pts',(7.98452790924092,31.5236177119233,-7.38646189178608));
#24877=CARTESIAN_POINT('Ctrl Pts',(7.98884729936329,31.5730321441085,-8.42190857812903));
#24878=CARTESIAN_POINT('Ctrl Pts',(7.59881305327393,31.6796302915114,-10.4599186239401));
#24879=CARTESIAN_POINT('Ctrl Pts',(7.19925811072238,31.7343407022857,-11.4411259814758));
#24880=CARTESIAN_POINT('Ctrl Pts',(6.05469257606037,31.8378705213091,-13.1716639298901));
#24881=CARTESIAN_POINT('Ctrl Pts',(5.32841029609977,31.889549405654,-13.9094359049476));
#24882=CARTESIAN_POINT('Ctrl Pts',(3.62798333001476,31.9961823518139,-15.0727650575699));
#24883=CARTESIAN_POINT('Ctrl Pts',(2.66808101180657,32.0468545356208,-15.4843950802912));
#24884=CARTESIAN_POINT('Ctrl Pts',(1.11053836543475,32.127499557725,-15.8167122830523));
#24885=CARTESIAN_POINT('Ctrl Pts',(0.555369956406371,32.1562445610946,-15.875));
#24886=CARTESIAN_POINT('Ctrl Pts',(1.24483756636096E-13,32.1850000000001,
-15.875));
#24887=CARTESIAN_POINT('Origin',(0.,-18.001,-7.93750000000004));
#24888=CARTESIAN_POINT('',(1.4501979134028E-14,35.0425000069372,-15.875));
#24889=CARTESIAN_POINT('',(-1.66564366207583E-15,34.7250000000001,-15.875));
#24890=CARTESIAN_POINT('',(-9.72063396823211E-16,-18.001,-15.875));
#24891=CARTESIAN_POINT('Ctrl Pts',(-9.99200722162641E-15,35.0425000069372,
-15.875));
#24892=CARTESIAN_POINT('Ctrl Pts',(0.970090933462564,34.9922715236566,-15.875));
#24893=CARTESIAN_POINT('Ctrl Pts',(1.93248681409951,34.9437065644586,-15.6971471683423));
#24894=CARTESIAN_POINT('Ctrl Pts',(3.81822285928236,34.8427334070056,-14.9748445200943));
#24895=CARTESIAN_POINT('Ctrl Pts',(4.71329600152565,34.7880367669905,-14.4095741740582));
#24896=CARTESIAN_POINT('Ctrl Pts',(6.21605595886414,34.6815544612065,-12.9791294950926));
#24897=CARTESIAN_POINT('Ctrl Pts',(6.81519863680074,34.6321037804164,-12.1339790477124));
#24898=CARTESIAN_POINT('Ctrl Pts',(7.66110176306296,34.5261202464978,-10.2565710316361));
#24899=CARTESIAN_POINT('Ctrl Pts',(7.89755691956149,34.472331596896,-9.24108798867198));
#24900=CARTESIAN_POINT('Ctrl Pts',(7.96862631735271,34.3688680419953,-7.16309565896684));
#24901=CARTESIAN_POINT('Ctrl Pts',(7.79726863331709,34.3157805716978,-6.12047324327451));
#24902=CARTESIAN_POINT('Ctrl Pts',(7.06808748209868,34.2087269605643,-4.18340938579211));
#24903=CARTESIAN_POINT('Ctrl Pts',(6.5257636328328,34.1588522707425,-3.30441334610998));
#24904=CARTESIAN_POINT('Ctrl Pts',(5.12486611018882,34.0539998585826,-1.78732241538885));
#24905=CARTESIAN_POINT('Ctrl Pts',(4.27441882470329,33.9995451690497,-1.16857990293053));
#24906=CARTESIAN_POINT('Ctrl Pts',(2.3913441993438,33.8941911946945,-0.298668390678644));
#24907=CARTESIAN_POINT('Ctrl Pts',(1.37834973008372,33.8438669417104,-0.0526791921381577));
#24908=CARTESIAN_POINT('Ctrl Pts',(-0.679103325210624,33.7373380145512,
0.0372729376288422));
#24909=CARTESIAN_POINT('Ctrl Pts',(-1.70386196214072,33.6851246449656,-0.117350434261928));
#24910=CARTESIAN_POINT('Ctrl Pts',(-3.66013477795052,33.5819073436672,-0.816306061666204));
#24911=CARTESIAN_POINT('Ctrl Pts',(-4.5696032899542,33.527178784434,-1.36281168890308));
#24912=CARTESIAN_POINT('Ctrl Pts',(-6.1038472063139,33.4203636326017,-2.76085913608331));
#24913=CARTESIAN_POINT('Ctrl Pts',(-6.7206167227976,33.3709808813071,-3.59148092125172));
#24914=CARTESIAN_POINT('Ctrl Pts',(-7.60850475049445,33.2652377919484,-5.45036439257499));
#24915=CARTESIAN_POINT('Ctrl Pts',(-7.86766437450084,33.2112432397888,-6.46265166913726));
#24916=CARTESIAN_POINT('Ctrl Pts',(-7.98317485724195,33.1072575635412,-8.53680718435962));
#24917=CARTESIAN_POINT('Ctrl Pts',(-7.83559071200281,33.0550463207417,-9.57881433209888));
#24918=CARTESIAN_POINT('Ctrl Pts',(-7.15237728567606,32.9481081623779,-11.5284694538581));
#24919=CARTESIAN_POINT('Ctrl Pts',(-6.63021560611076,32.8978139630681,-12.4198874319169));
#24920=CARTESIAN_POINT('Ctrl Pts',(-5.2626962307764,32.7933376145242,-13.9705626696936));
#24921=CARTESIAN_POINT('Ctrl Pts',(-4.4244432838421,32.7387734553081,-14.6096862254101));
#24922=CARTESIAN_POINT('Ctrl Pts',(-2.56119712677316,32.6329985178308,-15.5207213710765));
#24923=CARTESIAN_POINT('Ctrl Pts',(-1.55655463281693,32.5830938725771,-15.788746995707));
#24924=CARTESIAN_POINT('Ctrl Pts',(-0.35252362084797,32.5207526533491,-15.8691352102942));
#24925=CARTESIAN_POINT('Ctrl Pts',(-0.176167739284417,32.5116214594135,
-15.875));
#24926=CARTESIAN_POINT('Ctrl Pts',(-5.48172618408671E-15,32.5025000069372,
-15.875));
#24927=CARTESIAN_POINT('Ctrl Pts',(1.19348975147204E-13,32.1850000000001,
-15.875));
#24928=CARTESIAN_POINT('Ctrl Pts',(-0.479821973824826,32.2098437843904,
-15.875));
#24929=CARTESIAN_POINT('Ctrl Pts',(-0.95979439088142,32.2346953582927,-15.8314925177406));
#24930=CARTESIAN_POINT('Ctrl Pts',(-2.44052190888781,32.3113631167635,-15.559514895666));
#24931=CARTESIAN_POINT('Ctrl Pts',(-3.4018624930967,32.3610302127626,-15.1817084661653));
#24932=CARTESIAN_POINT('Ctrl Pts',(-5.14999927583338,32.4681524913806,-14.067967661525));
#24933=CARTESIAN_POINT('Ctrl Pts',(-5.91441854190448,32.521881254785,-13.3342017457131));
#24934=CARTESIAN_POINT('Ctrl Pts',(-7.10334001050634,32.6249856054144,-11.6267161052087));
#24935=CARTESIAN_POINT('Ctrl Pts',(-7.52209463175434,32.6786253221975,-10.6734901993414));
#24936=CARTESIAN_POINT('Ctrl Pts',(-7.97067507649972,32.7847494926242,-8.66412824505769));
#24937=CARTESIAN_POINT('Ctrl Pts',(-7.99771737810506,32.834308928385,-7.6273558962722));
#24938=CARTESIAN_POINT('Ctrl Pts',(-7.65190541526759,32.9405579782968,-5.58206645029218));
#24939=CARTESIAN_POINT('Ctrl Pts',(-7.27491157723585,32.9952194098341,-4.5945231904542));
#24940=CARTESIAN_POINT('Ctrl Pts',(-6.1713828811108,33.0991910219691,-2.84167985969742));
#24941=CARTESIAN_POINT('Ctrl Pts',(-5.46287826007856,33.1501742885371,-2.08853424230292));
#24942=CARTESIAN_POINT('Ctrl Pts',(-3.78793941754756,33.2569517942899,-0.885373730014236));
#24943=CARTESIAN_POINT('Ctrl Pts',(-2.83443565213759,33.3082411768288,-0.451051786516673));
#24944=CARTESIAN_POINT('Ctrl Pts',(-0.814360119641338,33.4128348047143,
0.02603283564326));
#24945=CARTESIAN_POINT('Ctrl Pts',(0.23273205517928,33.4670501880172,0.0641746315103381));
#24946=CARTESIAN_POINT('Ctrl Pts',(2.268387340936,33.5724504901527,-0.262433230432161));
#24947=CARTESIAN_POINT('Ctrl Pts',(3.23842845507517,33.6219142003453,-0.618703479819044));
#24948=CARTESIAN_POINT('Ctrl Pts',(5.0150716781271,33.7291050467692,-1.69546154969738));
#24949=CARTESIAN_POINT('Ctrl Pts',(5.79848012757925,33.7838360999378,-2.41555591413844));
#24950=CARTESIAN_POINT('Ctrl Pts',(7.02387583415542,33.8864233216061,-4.09977430173718));
#24951=CARTESIAN_POINT('Ctrl Pts',(7.46184247993154,33.9398022270509,-5.04191207434748));
#24952=CARTESIAN_POINT('Ctrl Pts',(7.95362461121147,34.0461177491235,-7.04112281968223));
#24953=CARTESIAN_POINT('Ctrl Pts',(8.00272599438934,34.0959286274556,-8.0790886997892));
#24954=CARTESIAN_POINT('Ctrl Pts',(7.69962425601701,34.2018141938604,-10.1308741045105));
#24955=CARTESIAN_POINT('Ctrl Pts',(7.3444580136891,34.2564037662479,-11.1240503017925));
#24956=CARTESIAN_POINT('Ctrl Pts',(6.28067601693568,34.3607707854692,-12.8978378399292));
#24957=CARTESIAN_POINT('Ctrl Pts',(5.58927625729154,34.4112031799623,-13.6656632453394));
#24958=CARTESIAN_POINT('Ctrl Pts',(3.93898630872078,34.5181070255036,-14.9069013469801));
#24959=CARTESIAN_POINT('Ctrl Pts',(2.99174533661782,34.5700961395091,-15.362963791741));
#24960=CARTESIAN_POINT('Ctrl Pts',(1.33422262317561,34.6559178383083,-15.7907462141402));
#24961=CARTESIAN_POINT('Ctrl Pts',(0.667699158686123,34.6904284821436,-15.875));
#24962=CARTESIAN_POINT('Ctrl Pts',(1.29063426612674E-14,34.7250000000001,
-15.875));
#24963=CARTESIAN_POINT('Origin',(0.,-18.001,-7.93750000000004));
#24964=CARTESIAN_POINT('',(-5.69020212634203E-15,37.5825000069372,-15.875));
#24965=CARTESIAN_POINT('',(7.63247416915985E-15,37.2650000000001,-15.875));
#24966=CARTESIAN_POINT('',(-9.72063396823211E-16,-18.001,-15.875));
#24967=CARTESIAN_POINT('Ctrl Pts',(-6.14559781626452E-14,37.5825000069372,
-15.875));
#24968=CARTESIAN_POINT('Ctrl Pts',(0.0648007681039002,37.5791448118879,
-15.875));
#24969=CARTESIAN_POINT('Ctrl Pts',(0.12963596222447,37.5757878343597,-15.8742064650826));
#24970=CARTESIAN_POINT('Ctrl Pts',(1.21770299726839,37.5194508921281,-15.8475377204892));
#24971=CARTESIAN_POINT('Ctrl Pts',(2.22646116209439,37.4691901787736,-15.624785921622));
#24972=CARTESIAN_POINT('Ctrl Pts',(4.12233564784132,37.364686501604,-14.8004311361088));
#24973=CARTESIAN_POINT('Ctrl Pts',(4.98813466023159,37.3101291116282,-14.1994439118828));
#24974=CARTESIAN_POINT('Ctrl Pts',(6.42806682210644,37.204382590406,-12.7067007433853));
#24975=CARTESIAN_POINT('Ctrl Pts',(6.99215060066927,37.1544526769673,-11.8330247778842));
#24976=CARTESIAN_POINT('Ctrl Pts',(7.75433965280672,37.0480776373944,-9.92046591662647));
#24977=CARTESIAN_POINT('Ctrl Pts',(7.94574814392369,36.9950319317637,-8.90007367658115));
#24978=CARTESIAN_POINT('Ctrl Pts',(7.92850355379243,36.8922703274921,-6.81884745579795));
#24979=CARTESIAN_POINT('Ctrl Pts',(7.71036723229586,36.8375358499281,-5.77820487914458));
#24980=CARTESIAN_POINT('Ctrl Pts',(6.89216633471838,36.7304415224441,-3.86923844409522));
#24981=CARTESIAN_POINT('Ctrl Pts',(6.31035446161657,36.6810175743866,-3.01488271303926));
#24982=CARTESIAN_POINT('Ctrl Pts',(4.84503125674973,36.5755206401467,-1.56528829467365));
#24983=CARTESIAN_POINT('Ctrl Pts',(3.97191179476745,36.5213606287323,-0.987433946974345));
#24984=CARTESIAN_POINT('Ctrl Pts',(2.05118100985973,36.4169255320887,-0.199544354491347));
#24985=CARTESIAN_POINT('Ctrl Pts',(1.02182551332679,36.3654071560936,0.00222508803780422));
#24986=CARTESIAN_POINT('Ctrl Pts',(-1.04129465620275,36.2585848022639,-0.00223011638187775));
#24987=CARTESIAN_POINT('Ctrl Pts',(-2.05539139111777,36.2078039963006,-0.202636926533077));
#24988=CARTESIAN_POINT('Ctrl Pts',(-3.97169591767539,36.1036931728616,-0.985963708951519));
#24989=CARTESIAN_POINT('Ctrl Pts',(-4.85226215942494,36.0490537047291,-1.56932252571176));
#24990=CARTESIAN_POINT('Ctrl Pts',(-6.32370333397671,35.9429265413702,-3.03120447219226));
#24991=CARTESIAN_POINT('Ctrl Pts',(-6.90535534830421,35.893293126359,-3.89064945096875));
#24992=CARTESIAN_POINT('Ctrl Pts',(-7.70949343749074,35.7871033330414,-5.78581635903722));
#24993=CARTESIAN_POINT('Ctrl Pts',(-7.92346919040345,35.733542764425,-6.80397165270648));
#24994=CARTESIAN_POINT('Ctrl Pts',(-7.95045596877978,35.6306243345731,-8.88521717713868));
#24995=CARTESIAN_POINT('Ctrl Pts',(-7.75532755669859,35.5765526174918,-9.92829577969207));
#24996=CARTESIAN_POINT('Ctrl Pts',(-6.98027194086661,35.4693980056103,-11.8525051908394));
#24997=CARTESIAN_POINT('Ctrl Pts',(-6.41784131115587,35.4198145663908,-12.719006969005));
#24998=CARTESIAN_POINT('Ctrl Pts',(-4.9839729914452,35.3146184605473,-14.2020106446483));
#24999=CARTESIAN_POINT('Ctrl Pts',(-4.12177453714119,35.2603004795952,-14.8000870636612));
#25000=CARTESIAN_POINT('Ctrl Pts',(-2.21932381032028,35.1553986501384,-15.6284729951544));
#25001=CARTESIAN_POINT('Ctrl Pts',(-1.1979951139365,35.1045287049437,-15.8521240368318));
#25002=CARTESIAN_POINT('Ctrl Pts',(-0.108359865597093,35.0481105651948,
-15.8744455157375));
#25003=CARTESIAN_POINT('Ctrl Pts',(-0.0541678346537001,35.0453046596593,
-15.875));
#25004=CARTESIAN_POINT('Ctrl Pts',(-4.55229467871315E-15,35.0425000069372,
-15.875));
#25005=CARTESIAN_POINT('Ctrl Pts',(1.11022302462516E-15,34.7250000000001,
-15.875));
#25006=CARTESIAN_POINT('Ctrl Pts',(-0.363509860640991,34.7438214819125,
-15.875));
#25007=CARTESIAN_POINT('Ctrl Pts',(-0.727368191051986,34.7626610065743,
-15.850029402379));
#25008=CARTESIAN_POINT('Ctrl Pts',(-2.10401211480627,34.8339396196637,-15.6593567340553));
#25009=CARTESIAN_POINT('Ctrl Pts',(-3.08223203909142,34.8833245093867,-15.3235523334587));
#25010=CARTESIAN_POINT('Ctrl Pts',(-4.87999195226312,34.9902273372992,-14.2853226623512));
#25011=CARTESIAN_POINT('Ctrl Pts',(-5.67697430303928,35.0449600603399,-13.5838563013009));
#25012=CARTESIAN_POINT('Ctrl Pts',(-6.93653105482265,35.1480413436088,-11.9304225865429));
#25013=CARTESIAN_POINT('Ctrl Pts',(-7.39453834961942,35.2004969651798,-11.0001859168604));
#25014=CARTESIAN_POINT('Ctrl Pts',(-7.93179481923721,35.3069802201514,-9.01234444706242));
#25015=CARTESIAN_POINT('Ctrl Pts',(-8.00421237791695,35.3571734658315,-7.97322362338979));
#25016=CARTESIAN_POINT('Ctrl Pts',(-7.74599857552462,35.462649286388,-5.91517415017933));
#25017=CARTESIAN_POINT('Ctrl Pts',(-7.41379961298889,35.5171375939901,-4.91659186403143));
#25018=CARTESIAN_POINT('Ctrl Pts',(-6.39191085395918,35.6218872236836,-3.12142253291469));
#25019=CARTESIAN_POINT('Ctrl Pts',(-5.71843033335381,35.6718672305716,-2.33833386040319));
#25020=CARTESIAN_POINT('Ctrl Pts',(-4.09409882353876,35.7788897281313,-1.05746834187355));
#25021=CARTESIAN_POINT('Ctrl Pts',(-3.15353713284373,35.8317190314962,-0.578733174653649));
#25022=CARTESIAN_POINT('Ctrl Pts',(-1.15239837642726,35.935332168267,-0.0163885496313035));
#25023=CARTESIAN_POINT('Ctrl Pts',(-0.112382454211418,35.9891811638186,
0.0662013203635666));
#25024=CARTESIAN_POINT('Ctrl Pts',(1.93329509262871,36.0951003894446,-0.170977548322487));
#25025=CARTESIAN_POINT('Ctrl Pts',(2.91988456334042,36.1445200830762,-0.485602244766304));
#25026=CARTESIAN_POINT('Ctrl Pts',(4.73884062868974,36.2510985537357,-1.48400012152621));
#25027=CARTESIAN_POINT('Ctrl Pts',(5.54932921408693,36.3058068135178,-2.16607292692184));
#25028=CARTESIAN_POINT('Ctrl Pts',(6.84347895779032,36.4093634168762,-3.78751163298749));
#25029=CARTESIAN_POINT('Ctrl Pts',(7.32189173198879,36.4609980264526,-4.70551888221592));
#25030=CARTESIAN_POINT('Ctrl Pts',(7.9055134476158,36.5676398241248,-6.68151497324313));
#25031=CARTESIAN_POINT('Ctrl Pts',(8.0017547186586,36.6183450548568,-7.72169504645281));
#25032=CARTESIAN_POINT('Ctrl Pts',(7.78911407750309,36.7233759385058,-9.78551658956596));
#25033=CARTESIAN_POINT('Ctrl Pts',(7.48024700718692,36.777734724559,-10.7890496106528));
#25034=CARTESIAN_POINT('Ctrl Pts',(6.50101684593399,36.8828384077115,-12.6052694942955));
#25035=CARTESIAN_POINT('Ctrl Pts',(5.84568059562513,36.9324900533354,-13.4036939864018));
#25036=CARTESIAN_POINT('Ctrl Pts',(4.24777912829267,37.0396180231976,-14.724402966992));
#25037=CARTESIAN_POINT('Ctrl Pts',(3.31411010317857,37.093405030739,-15.2259808346506));
#25038=CARTESIAN_POINT('Ctrl Pts',(1.55990245202554,37.1842327940314,-15.7596126746479));
#25039=CARTESIAN_POINT('Ctrl Pts',(0.781373958260331,37.2245427320836,-15.875));
#25040=CARTESIAN_POINT('Ctrl Pts',(6.1478599988618E-14,37.2650000000001,
-15.875));
#25041=CARTESIAN_POINT('Origin',(0.,-18.001,-7.93750000000004));
#25042=CARTESIAN_POINT('',(1.80380328987778E-15,40.1225000069372,-15.875));
#25043=CARTESIAN_POINT('',(1.84571486592551E-14,39.805,-15.875));
#25044=CARTESIAN_POINT('',(-9.72063396823211E-16,-18.001,-15.875));
#25045=CARTESIAN_POINT('Ctrl Pts',(5.9986737799278E-14,40.1225000069372,
-15.875));
#25046=CARTESIAN_POINT('Ctrl Pts',(0.185867297990525,40.1128763395597,-15.875));
#25047=CARTESIAN_POINT('Ctrl Pts',(0.371944385759047,40.103241809879,-15.8684716342223));
#25048=CARTESIAN_POINT('Ctrl Pts',(1.57889074635526,40.0407496423896,-15.7834306632627));
#25049=CARTESIAN_POINT('Ctrl Pts',(2.57638491518406,39.9911817245374,-15.5146893568303));
#25050=CARTESIAN_POINT('Ctrl Pts',(4.42832218354737,39.8859628737238,-14.6063608649745));
#25051=CARTESIAN_POINT('Ctrl Pts',(5.26242841254009,39.8316554417827,-13.9699654363925));
#25052=CARTESIAN_POINT('Ctrl Pts',(6.63580409260786,39.7267863109672,-12.4144445942834));
#25053=CARTESIAN_POINT('Ctrl Pts',(7.16280366634182,39.6758735707267,-11.5111784728837));
#25054=CARTESIAN_POINT('Ctrl Pts',(7.83653466399014,39.5691794174613,-9.56339745218134));
#25055=CARTESIAN_POINT('Ctrl Pts',(7.98079626566829,39.5178024314015,-8.53879810000055));
#25056=CARTESIAN_POINT('Ctrl Pts',(7.87048579900228,39.414086729212,-6.46843549020098));
#25057=CARTESIAN_POINT('Ctrl Pts',(7.60791398256985,39.3593933345895,-5.4430651721184));
#25058=CARTESIAN_POINT('Ctrl Pts',(6.70901558264553,39.2529355379743,-3.57324528354891));
#25059=CARTESIAN_POINT('Ctrl Pts',(6.08901666201518,39.2034756052062,-2.7431306233325));
#25060=CARTESIAN_POINT('Ctrl Pts',(4.5627511221141,39.0974762991203,-1.36090910126765));
#25061=CARTESIAN_POINT('Ctrl Pts',(3.66934538919467,39.0437031321698,-0.823687420761977));
#25062=CARTESIAN_POINT('Ctrl Pts',(1.71380952697431,38.9402775522919,-0.116873805681974));
#25063=CARTESIAN_POINT('Ctrl Pts',(0.668706479971726,38.8871236809561,0.0407489814137206));
#25064=CARTESIAN_POINT('Ctrl Pts',(-1.39902799814106,38.7800624116666,-0.057539562425789));
#25065=CARTESIAN_POINT('Ctrl Pts',(-2.40219030683038,38.7302126473264,-0.303329135149752));
#25066=CARTESIAN_POINT('Ctrl Pts',(-4.27637136753711,38.6253347448599,-1.16983872628206));
#25067=CARTESIAN_POINT('Ctrl Pts',(-5.12650815803909,38.5708888676778,-1.78871904048554));
#25068=CARTESIAN_POINT('Ctrl Pts',(-6.53338217014492,38.4655659817784,-3.3130429568106));
#25069=CARTESIAN_POINT('Ctrl Pts',(-7.07904785220948,38.4152071427341,-4.20149410445223));
#25070=CARTESIAN_POINT('Ctrl Pts',(-7.79724476709036,38.3086668457171,-6.13170283999069));
#25071=CARTESIAN_POINT('Ctrl Pts',(-7.965183003106,38.2565131010932,-7.15423708406995));
#25072=CARTESIAN_POINT('Ctrl Pts',(-7.90165369156493,38.1532618300973,-9.23036838493943));
#25073=CARTESIAN_POINT('Ctrl Pts',(-7.66135886518496,38.0985346504455,-10.2636630247046));
#25074=CARTESIAN_POINT('Ctrl Pts',(-6.80297851111757,37.9917420113679,-12.1534478313711));
#25075=CARTESIAN_POINT('Ctrl Pts',(-6.20224707983457,37.9423583482901,-12.995846776573));
#25076=CARTESIAN_POINT('Ctrl Pts',(-4.70655188507403,37.8365973253077,-14.412315216426));
#25077=CARTESIAN_POINT('Ctrl Pts',(-3.82317267607415,37.7826164241643,-14.9701629936973));
#25078=CARTESIAN_POINT('Ctrl Pts',(-1.94551186050395,37.6819123589154,-15.6947383580089));
#25079=CARTESIAN_POINT('Ctrl Pts',(-0.976631580980323,37.6330671458976,
-15.875));
#25080=CARTESIAN_POINT('Ctrl Pts',(-5.87030424270552E-14,37.5825000069372,
-15.875));
#25081=CARTESIAN_POINT('Ctrl Pts',(5.28743715477731E-14,37.2650000000001,
-15.875));
#25082=CARTESIAN_POINT('Ctrl Pts',(-0.246325470798439,37.2777540154896,
-15.875));
#25083=CARTESIAN_POINT('Ctrl Pts',(-0.492933725020677,37.2905226726808,
-15.8635338979502));
#25084=CARTESIAN_POINT('Ctrl Pts',(-1.76216030317954,37.3562395284532,-15.7448462700579));
#25085=CARTESIAN_POINT('Ctrl Pts',(-2.75701869450834,37.4058108170844,-15.4514028738958));
#25086=CARTESIAN_POINT('Ctrl Pts',(-4.59650542976917,37.5120390370243,-14.4927716462837));
#25087=CARTESIAN_POINT('Ctrl Pts',(-5.41994727147877,37.566696878774,-13.8301841142049));
#25088=CARTESIAN_POINT('Ctrl Pts',(-6.74791495111436,37.6706927887025,-12.2408569830228));
#25089=CARTESIAN_POINT('Ctrl Pts',(-7.24640490395248,37.7216400948249,-11.3349899794204));
#25090=CARTESIAN_POINT('Ctrl Pts',(-7.87570224164693,37.82842545482,-9.37091940849076));
#25091=CARTESIAN_POINT('Ctrl Pts',(-7.99546242012346,37.8797535284719,-8.32982170422263));
#25092=CARTESIAN_POINT('Ctrl Pts',(-7.82750474973192,37.9843199465854,-6.26091390886392));
#25093=CARTESIAN_POINT('Ctrl Pts',(-7.54151344243943,38.0385259457425,-5.25305081879688));
#25094=CARTESIAN_POINT('Ctrl Pts',(-6.60423189572394,38.1439432223175,-3.41683271158838));
#25095=CARTESIAN_POINT('Ctrl Pts',(-5.96665031585442,38.1933991011947,-2.60351775144321));
#25096=CARTESIAN_POINT('Ctrl Pts',(-4.39537345261552,38.3005734616406,-1.24463883631588));
#25097=CARTESIAN_POINT('Ctrl Pts',(-3.46923623280529,38.3553053237183,-0.720967191637942));
#25098=CARTESIAN_POINT('Ctrl Pts',(-1.48988927923936,38.4579230202483,-0.0734723203727779));
#25099=CARTESIAN_POINT('Ctrl Pts',(-0.458829348094782,38.5112431526314,
0.0532894238835631));
#25100=CARTESIAN_POINT('Ctrl Pts',(1.59470343952526,38.6175690997477,-0.0939780982895629));
#25101=CARTESIAN_POINT('Ctrl Pts',(2.59754266809464,38.667399587462,-0.366719226636373));
#25102=CARTESIAN_POINT('Ctrl Pts',(4.45645307465599,38.7732612712922,-1.28657234944641));
#25103=CARTESIAN_POINT('Ctrl Pts',(5.29201868124709,38.8278454869227,-1.93005372939396));
#25104=CARTESIAN_POINT('Ctrl Pts',(6.65228551138309,38.9322365117142,-3.48790765481004));
#25105=CARTESIAN_POINT('Ctrl Pts',(7.17008966563123,38.9826379953507,-4.38199638047202));
#25106=CARTESIAN_POINT('Ctrl Pts',(7.84337351461919,39.0895494003904,-6.33433452486375));
#25107=CARTESIAN_POINT('Ctrl Pts',(7.98582844272044,39.1415861421795,-7.37618898469444));
#25108=CARTESIAN_POINT('Ctrl Pts',(7.86068429551567,39.2456813681751,-9.44943901200891));
#25109=CARTESIAN_POINT('Ctrl Pts',(7.59659859145796,39.2997173356786,-10.4609667494475));
#25110=CARTESIAN_POINT('Ctrl Pts',(6.69962519227849,39.4054039973125,-12.3157522996759));
#25111=CARTESIAN_POINT('Ctrl Pts',(6.07903425107462,39.4547876391827,-13.1432083713512));
#25112=CARTESIAN_POINT('Ctrl Pts',(4.53797774525617,39.561671536427,-14.5341379436891));
#25113=CARTESIAN_POINT('Ctrl Pts',(3.62542075252794,39.6164035277038,-15.0765054126516));
#25114=CARTESIAN_POINT('Ctrl Pts',(1.78672925347056,39.7131060004465,-15.7232323347485));
#25115=CARTESIAN_POINT('Ctrl Pts',(0.896114797452721,39.7586017855968,-15.875));
#25116=CARTESIAN_POINT('Ctrl Pts',(7.2025718722557E-14,39.805,-15.875));
#25117=CARTESIAN_POINT('Origin',(0.,-18.001,-7.93750000000004));
#25118=CARTESIAN_POINT('',(-2.65762727771028E-14,42.6625000069372,-15.875));
#25119=CARTESIAN_POINT('',(-6.2616496713002E-9,42.3450000006485,-15.875));
#25120=CARTESIAN_POINT('',(-9.72063396823211E-16,-18.001,-15.875));
#25121=CARTESIAN_POINT('Ctrl Pts',(-1.21430643318376E-14,42.6625000069372,
-15.875));
#25122=CARTESIAN_POINT('Ctrl Pts',(0.300454544332103,42.6469433456635,-15.875));
#25123=CARTESIAN_POINT('Ctrl Pts',(0.60125822561139,42.6313686070956,-15.8579410296588));
#25124=CARTESIAN_POINT('Ctrl Pts',(1.91951584091607,42.5631130670159,-15.7073371473094));
#25125=CARTESIAN_POINT('Ctrl Pts',(2.90591665428349,42.5137278838793,-15.3947491935123));
#25126=CARTESIAN_POINT('Ctrl Pts',(4.7136267695739,42.4079488643821,-14.4071411162044));
#25127=CARTESIAN_POINT('Ctrl Pts',(5.51598669608921,42.3539819098442,-13.7382381235893));
#25128=CARTESIAN_POINT('Ctrl Pts',(6.82385615017907,42.2500682907801,-12.1239520873497));
#25129=CARTESIAN_POINT('Ctrl Pts',(7.31428406470129,42.1977404128448,-11.1921586784889));
#25130=CARTESIAN_POINT('Ctrl Pts',(7.9012607442347,42.0907851526947,-9.21088704799251));
#25131=CARTESIAN_POINT('Ctrl Pts',(7.99946203179922,42.0405577307008,-8.18253679286367));
#25132=CARTESIAN_POINT('Ctrl Pts',(7.79800018427309,41.9360265225012,-6.12523018922354));
#25133=CARTESIAN_POINT('Ctrl Pts',(7.4924218338955,41.8814761264338,-5.11673748152932));
#25134=CARTESIAN_POINT('Ctrl Pts',(6.514850757226,41.7757585515474,-3.28751193389603));
#25135=CARTESIAN_POINT('Ctrl Pts',(5.85685564858871,41.7258024157269,-2.4819637473802));
#25136=CARTESIAN_POINT('Ctrl Pts',(4.27128902936751,41.6194153347666,-1.16862157650717));
#25137=CARTESIAN_POINT('Ctrl Pts',(3.35932997630399,41.5664363295322,-0.672786206102429));
#25138=CARTESIAN_POINT('Ctrl Pts',(1.37395363649707,41.4636393247877,-0.0492519434039022));
#25139=CARTESIAN_POINT('Ctrl Pts',(0.31682951160224,41.4089045163267,0.0632246299822857));
#25140=CARTESIAN_POINT('Ctrl Pts',(-1.75115225875815,41.3018304429648,-0.128128031572477));
#25141=CARTESIAN_POINT('Ctrl Pts',(-2.74309856090656,41.2524130366757,-0.418972246627263));
#25142=CARTESIAN_POINT('Ctrl Pts',(-4.57302366092601,41.146896637977,-1.36737477531151));
#25143=CARTESIAN_POINT('Ctrl Pts',(-5.39130545400732,41.0927483743506,-2.02032068794153));
#25144=CARTESIAN_POINT('Ctrl Pts',(-6.73190329291471,40.9883463181676,-3.60560912888532));
#25145=CARTESIAN_POINT('Ctrl Pts',(-7.24061972766324,40.9367791529986,-4.52322227145597));
#25146=CARTESIAN_POINT('Ctrl Pts',(-7.87091814714441,40.829947725114,-6.48790309398654));
#25147=CARTESIAN_POINT('Ctrl Pts',(-7.99209826798352,40.7792070067401,-7.5144255662737));
#25148=CARTESIAN_POINT('Ctrl Pts',(-7.83612457682176,40.6750678728088,-9.57855012710422));
#25149=CARTESIAN_POINT('Ctrl Pts',(-7.55193763598935,40.6204332959951,-10.5957028239988));
#25150=CARTESIAN_POINT('Ctrl Pts',(-6.61358117058684,40.5143316941337,-12.4454685917169));
#25151=CARTESIAN_POINT('Ctrl Pts',(-5.9746255177841,40.4646813857368,-13.2633856477434));
#25152=CARTESIAN_POINT('Ctrl Pts',(-4.41865875031456,40.3584784649879,-14.6114173473667));
#25153=CARTESIAN_POINT('Ctrl Pts',(-3.51581695525116,40.3049346026081,-15.1281168683531));
#25154=CARTESIAN_POINT('Ctrl Pts',(-1.72020503836694,40.2112659530537,-15.7344517960849));
#25155=CARTESIAN_POINT('Ctrl Pts',(-0.862352704592977,40.1671501184995,
-15.875));
#25156=CARTESIAN_POINT('Ctrl Pts',(5.37070388162419E-14,40.1225000069372,
-15.875));
#25157=CARTESIAN_POINT('Ctrl Pts',(9.09688990802238E-14,39.805,-15.875));
#25158=CARTESIAN_POINT('Ctrl Pts',(-0.128923461931392,39.8116752813873,
-15.875));
#25159=CARTESIAN_POINT('Ctrl Pts',(-0.257961433384957,39.818356491744,-15.8718590127514));
#25160=CARTESIAN_POINT('Ctrl Pts',(-1.41780723665423,39.8784099295488,-15.8152422530517));
#25161=CARTESIAN_POINT('Ctrl Pts',(-2.42896253760847,39.9286309487171,-15.5643717670732));
#25162=CARTESIAN_POINT('Ctrl Pts',(-4.30770635463342,40.0340803549818,-14.6853636882796));
#25163=CARTESIAN_POINT('Ctrl Pts',(-5.15550411383657,40.0885615010144,-14.0621051029345));
#25164=CARTESIAN_POINT('Ctrl Pts',(-6.54908111448641,40.1933338099745,-12.5375703846111));
#25165=CARTESIAN_POINT('Ctrl Pts',(-7.08696717242735,40.2432899324377,-11.6558310944197));
#25166=CARTESIAN_POINT('Ctrl Pts',(-7.80602747190267,40.3503193264008,-9.71597056259306));
#25167=CARTESIAN_POINT('Ctrl Pts',(-7.97214689114645,40.4032043066804,-8.67347038615789));
#25168=CARTESIAN_POINT('Ctrl Pts',(-7.89131535184402,40.506784913823,-6.59627293232724));
#25169=CARTESIAN_POINT('Ctrl Pts',(-7.64987601671947,40.5606208742748,-5.58144858297681));
#25170=CARTESIAN_POINT('Ctrl Pts',(-6.79474000294826,40.6665543857725,-3.70805634326503));
#25171=CARTESIAN_POINT('Ctrl Pts',(-6.19172517110699,40.7159800649546,-2.86608687083622));
#25172=CARTESIAN_POINT('Ctrl Pts',(-4.68204147809769,40.8225376748708,-1.44269753865027));
#25173=CARTESIAN_POINT('Ctrl Pts',(-3.78378584066279,40.8772435685726,-0.881503462017499));
#25174=CARTESIAN_POINT('Ctrl Pts',(-1.84302089740972,40.980828303655,-0.149129868455843));
#25175=CARTESIAN_POINT('Ctrl Pts',(-0.822435479458738,41.0324166861016,
0.0236067096783087));
#25176=CARTESIAN_POINT('Ctrl Pts',(1.23737684193968,41.1390677691886,-0.029027715532643));
#25177=CARTESIAN_POINT('Ctrl Pts',(2.25689579584603,41.1898082845221,-0.25756096921839));
#25178=CARTESIAN_POINT('Ctrl Pts',(4.15517361440018,41.2948110684688,-1.09500759847268));
#25179=CARTESIAN_POINT('Ctrl Pts',(5.0148559220807,41.3491610847678,-1.69759981986668));
#25180=CARTESIAN_POINT('Ctrl Pts',(6.44159243080683,41.4542852588518,-3.18805604346756));
#25181=CARTESIAN_POINT('Ctrl Pts',(6.99965655552302,41.5039210909783,-4.05728027463741));
#25182=CARTESIAN_POINT('Ctrl Pts',(7.76474742221403,41.6110550038067,-5.98430708342086));
#25183=CARTESIAN_POINT('Ctrl Pts',(7.95470864438124,41.6649037667633,-7.02730052722785));
#25184=CARTESIAN_POINT('Ctrl Pts',(7.91816984828705,41.7679426179726,-9.10788786739275));
#25185=CARTESIAN_POINT('Ctrl Pts',(7.69932733321596,41.8215546040985,-10.1255060142777));
#25186=CARTESIAN_POINT('Ctrl Pts',(6.8861293697943,41.9277024299275,-12.0168769367812));
#25187=CARTESIAN_POINT('Ctrl Pts',(6.30068628876214,41.9772866121413,-12.8732340780505));
#25188=CARTESIAN_POINT('Ctrl Pts',(4.82245152923863,42.0834928057278,-14.3283622475923));
#25189=CARTESIAN_POINT('Ctrl Pts',(3.93872346358835,42.1381467768533,-14.9078457292674));
#25190=CARTESIAN_POINT('Ctrl Pts',(2.02470881339383,42.2418073226377,-15.6795289453528));
#25191=CARTESIAN_POINT('Ctrl Pts',(1.01703327273241,42.292340979105,-15.8750000016047));
#25192=CARTESIAN_POINT('Ctrl Pts',(-1.25233615144715E-8,42.3450000006485,
-15.875));
#25193=CARTESIAN_POINT('Origin',(0.,-18.001,-7.93750000000004));
#25194=CARTESIAN_POINT('',(-2.92477469301071E-14,45.2025000069372,-15.875));
#25195=CARTESIAN_POINT('',(8.46514143762872E-15,44.885,-15.875));
#25196=CARTESIAN_POINT('',(-9.72063396823211E-16,-18.001,-15.875));
#25197=CARTESIAN_POINT('Ctrl Pts',(-1.83186799063151E-14,45.2025000069372,
-15.875));
#25198=CARTESIAN_POINT('Ctrl Pts',(0.414093089374723,45.1810594727575,-15.875));
#25199=CARTESIAN_POINT('Ctrl Pts',(0.828501962723747,45.1596025882034,-15.842596332934));
#25200=CARTESIAN_POINT('Ctrl Pts',(2.25518995910534,45.0857328387799,-15.6170597446468));
#25201=CARTESIAN_POINT('Ctrl Pts',(3.2301180397819,45.0360649594813,-15.2606023136635));
#25202=CARTESIAN_POINT('Ctrl Pts',(4.99133973839858,44.9298489672139,-14.19465028386));
#25203=CARTESIAN_POINT('Ctrl Pts',(5.76057075917527,44.8763220528392,-13.4946081896136));
#25204=CARTESIAN_POINT('Ctrl Pts',(7.0009989017113,44.7734817570966,-11.8227646179266));
#25205=CARTESIAN_POINT('Ctrl Pts',(7.45357972913763,44.7192638026932,-10.8622051736005));
#25206=CARTESIAN_POINT('Ctrl Pts',(7.95130601089794,44.6120962317578,-8.84762283372994));
#25207=CARTESIAN_POINT('Ctrl Pts',(8.00230032536853,44.5625433313465,-7.81578750250976));
#25208=CARTESIAN_POINT('Ctrl Pts',(7.70742658653592,44.4573017101486,-5.77440556374169));
#25209=CARTESIAN_POINT('Ctrl Pts',(7.35841791020113,44.4030050483682,-4.78517692857907));
#25210=CARTESIAN_POINT('Ctrl Pts',(6.30061393659308,44.298169040757,-2.99992304014986));
#25211=CARTESIAN_POINT('Ctrl Pts',(5.60300453270788,44.2472125238532,-2.22052955071996));
#25212=CARTESIAN_POINT('Ctrl Pts',(3.9565996009202,44.1405079699132,-0.980492544419229));
#25213=CARTESIAN_POINT('Ctrl Pts',(3.02607306041202,44.0891812569913,-0.52822382645339));
#25214=CARTESIAN_POINT('Ctrl Pts',(1.02234021118214,43.9854338056496,0.00335437628450272));
#25215=CARTESIAN_POINT('Ctrl Pts',(-0.03391822241176,43.930743820163,0.0688139935690083));
#25216=CARTESIAN_POINT('Ctrl Pts',(-2.08951685814976,43.8243109094478,-0.21145543413736));
#25217=CARTESIAN_POINT('Ctrl Pts',(-3.07018109632898,43.7748410382994,-0.546165898899786));
#25218=CARTESIAN_POINT('Ctrl Pts',(-4.85472481487504,43.6688259661318,-1.5734160504032));
#25219=CARTESIAN_POINT('Ctrl Pts',(-5.6405408372536,43.6150685612002,-2.25820435184308));
#25220=CARTESIAN_POINT('Ctrl Pts',(-6.91463230239517,43.5116814811785,-3.9016806791066));
#25221=CARTESIAN_POINT('Ctrl Pts',(-7.3861361833161,43.4584599442885,-4.84795809196937));
#25222=CARTESIAN_POINT('Ctrl Pts',(-7.92841842210969,43.3513910090069,-6.84606028214751));
#25223=CARTESIAN_POINT('Ctrl Pts',(-8.00295760332611,43.3015657794211,-7.8762028670668));
#25224=CARTESIAN_POINT('Ctrl Pts',(-7.75465683012312,43.1966622791342,-9.9258508957005));
#25225=CARTESIAN_POINT('Ctrl Pts',(-7.42721296297431,43.1422254493468,-10.9249328212549));
#25226=CARTESIAN_POINT('Ctrl Pts',(-6.40936083873474,43.036934144788,-12.7324137865624));
#25227=CARTESIAN_POINT('Ctrl Pts',(-5.73159127342935,42.9865397015636,-13.5249806950076));
#25228=CARTESIAN_POINT('Ctrl Pts',(-4.11560421824636,42.8799879692098,-14.8018628753267));
#25229=CARTESIAN_POINT('Ctrl Pts',(-3.1943453937713,42.8278939083433,-15.2759982468382));
#25230=CARTESIAN_POINT('Ctrl Pts',(-1.48929540753733,42.7396113857753,-15.7699023313494));
#25231=CARTESIAN_POINT('Ctrl Pts',(-0.745723087441236,42.7011113765908,
-15.875));
#25232=CARTESIAN_POINT('Ctrl Pts',(-5.41233724504764E-15,42.6625000069372,
-15.875));
#25233=CARTESIAN_POINT('Ctrl Pts',(-1.2523352834363E-8,42.3450000006485,
-15.875));
#25234=CARTESIAN_POINT('Ctrl Pts',(-0.00718283073825684,42.3453719060567,
-15.8749999999887));
#25235=CARTESIAN_POINT('Ctrl Pts',(-0.0143661199379798,42.3457438358511,
-15.8749902501427));
#25236=CARTESIAN_POINT('Ctrl Pts',(-1.05976660879513,42.3998716285815,-15.8721520368392));
#25237=CARTESIAN_POINT('Ctrl Pts',(-2.08740291424895,42.4512408187044,-15.6656635511861));
#25238=CARTESIAN_POINT('Ctrl Pts',(-4.00424958390844,42.5557785175246,-14.8690566104206));
#25239=CARTESIAN_POINT('Ctrl Pts',(-4.87506285028589,42.6099745573722,-14.2868442275217));
#25240=CARTESIAN_POINT('Ctrl Pts',(-6.3336727297779,42.7154095731031,-12.8300442398946));
#25241=CARTESIAN_POINT('Ctrl Pts',(-6.91133069430021,42.7648576448598,-11.9730766733429));
#25242=CARTESIAN_POINT('Ctrl Pts',(-7.72065890152763,42.8720145680178,-10.0599561659786));
#25243=CARTESIAN_POINT('Ctrl Pts',(-7.93389431393028,42.9267471830165,-9.01775901144047));
#25244=CARTESIAN_POINT('Ctrl Pts',(-7.94093188920756,43.0293967969897,-6.93549057135042));
#25245=CARTESIAN_POINT('Ctrl Pts',(-7.74434012355705,43.0826556176578,-5.91558444175416));
#25246=CARTESIAN_POINT('Ctrl Pts',(-6.97244712715683,43.1889924725656,-4.00695401748261));
#25247=CARTESIAN_POINT('Ctrl Pts',(-6.40430688532385,43.2388440334976,-3.13655229747144));
#25248=CARTESIAN_POINT('Ctrl Pts',(-4.95709627578438,43.344680517238,-1.65087104682534));
#25249=CARTESIAN_POINT('Ctrl Pts',(-4.08787156469548,43.3992590024194,-1.05390574198236));
#25250=CARTESIAN_POINT('Ctrl Pts',(-2.18725613219509,43.5036751134421,-0.238953575351402));
#25251=CARTESIAN_POINT('Ctrl Pts',(-1.17726529609476,43.5540446315884,-0.0213287807175966));
#25252=CARTESIAN_POINT('Ctrl Pts',(0.887727052590154,43.6609639214022,0.0186985187400757));
#25253=CARTESIAN_POINT('Ctrl Pts',(1.9231168137452,43.7130511158005,-0.1663580163584));
#25254=CARTESIAN_POINT('Ctrl Pts',(3.85734793065473,43.8171144439488,-0.923450354424346));
#25255=CARTESIAN_POINT('Ctrl Pts',(4.73841970608408,43.8711384211649,-1.48588944352097));
#25256=CARTESIAN_POINT('Ctrl Pts',(6.22720874915739,43.9768417410447,-2.90996736593318));
#25257=CARTESIAN_POINT('Ctrl Pts',(6.82361929704801,44.0262245421741,-3.75510591832266));
#25258=CARTESIAN_POINT('Ctrl Pts',(7.67285742027115,44.1330884659885,-5.64930882929789));
#25259=CARTESIAN_POINT('Ctrl Pts',(7.90811583243183,44.1878195838756,-6.68431987487908));
#25260=CARTESIAN_POINT('Ctrl Pts',(7.96110460463708,44.2909619682184,-8.76166479094792));
#25261=CARTESIAN_POINT('Ctrl Pts',(7.78782588199072,44.3433080827685,-9.7837200503708));
#25262=CARTESIAN_POINT('Ctrl Pts',(7.05961136102939,44.4498118828499,-11.7099327075577));
#25263=CARTESIAN_POINT('Ctrl Pts',(6.50974743990282,44.5000625170366,-12.5950293995893));
#25264=CARTESIAN_POINT('Ctrl Pts',(5.09533745588943,44.6054841178605,-14.1122245346181));
#25265=CARTESIAN_POINT('Ctrl Pts',(4.24161592094833,44.6599576487681,-14.7270795228757));
#25266=CARTESIAN_POINT('Ctrl Pts',(2.36246672704688,44.7647535910512,-15.5840580016538));
#25267=CARTESIAN_POINT('Ctrl Pts',(1.35802910142151,44.814685208198,-15.8246308207638));
#25268=CARTESIAN_POINT('Ctrl Pts',(0.22371140399614,44.8734168750292,-15.8726375525265));
#25269=CARTESIAN_POINT('Ctrl Pts',(0.111809721412583,44.8792108182554,-15.875));
#25270=CARTESIAN_POINT('Ctrl Pts',(-1.18655085756814E-14,44.885,-15.875));
#25271=CARTESIAN_POINT('Origin',(0.,-18.001,-7.93750000000004));
#25272=CARTESIAN_POINT('',(6.78245966593122E-15,47.7425000069373,-15.875));
#25273=CARTESIAN_POINT('',(1.23509220238168E-14,47.425,-15.875));
#25274=CARTESIAN_POINT('',(-9.72063396823211E-16,-18.001,-15.875));
#25275=CARTESIAN_POINT('Ctrl Pts',(1.346145417358E-14,47.7425000069373,
-15.875));
#25276=CARTESIAN_POINT('Ctrl Pts',(0.536131078723344,47.7147407010877,-15.875));
#25277=CARTESIAN_POINT('Ctrl Pts',(1.07217525151894,47.686985894974,-15.8206810031299));
#25278=CARTESIAN_POINT('Ctrl Pts',(2.60215309102455,47.6077680982907,-15.5058499602607));
#25279=CARTESIAN_POINT('Ctrl Pts',(3.55518708976509,47.5577948449748,-15.1076985008461));
#25280=CARTESIAN_POINT('Ctrl Pts',(5.27582292987373,47.4507704060872,-13.9593207328677));
#25281=CARTESIAN_POINT('Ctrl Pts',(6.022115217456,47.3979255158128,-13.2129642659173));
#25282=CARTESIAN_POINT('Ctrl Pts',(7.17598098299624,47.2943215013235,-11.4839414226786));
#25283=CARTESIAN_POINT('Ctrl Pts',(7.5762594799151,47.2404761561679,-10.5205364658375));
#25284=CARTESIAN_POINT('Ctrl Pts',(7.98361143601375,47.1345529072572,-8.50185877341769));
#25285=CARTESIAN_POINT('Ctrl Pts',(7.98965182749404,47.0851315780006,-7.46630839809705));
#25286=CARTESIAN_POINT('Ctrl Pts',(7.60565637182131,46.9792981093663,-5.44186492991381));
#25287=CARTESIAN_POINT('Ctrl Pts',(7.21598333391762,46.9253452773936,-4.47283126405295));
#25288=CARTESIAN_POINT('Ctrl Pts',(6.08212765812418,46.821468256998,-2.73176268627033));
#25289=CARTESIAN_POINT('Ctrl Pts',(5.34609413436768,46.7690805884849,-1.97835371905176));
#25290=CARTESIAN_POINT('Ctrl Pts',(3.64105459911015,46.6621167900168,-0.810502013748309));
#25291=CARTESIAN_POINT('Ctrl Pts',(2.69273834198521,46.6119221560619,-0.400886571937467));
#25292=CARTESIAN_POINT('Ctrl Pts',(0.67333747039778,46.5073634601534,0.0399305255073528));
#25293=CARTESIAN_POINT('Ctrl Pts',(-0.380086693244262,46.4528202249105,
0.0592665995938344));
#25294=CARTESIAN_POINT('Ctrl Pts',(-2.42130517369179,46.347131876756,-0.308390799253155));
#25295=CARTESIAN_POINT('Ctrl Pts',(-3.39032224405438,46.2971487774006,-0.686865161060566));
#25296=CARTESIAN_POINT('Ctrl Pts',(-5.12757382038213,46.190749656441,-1.79182651200148));
#25297=CARTESIAN_POINT('Ctrl Pts',(-5.87969960599913,46.1378370944241,-2.50703017682195));
#25298=CARTESIAN_POINT('Ctrl Pts',(-7.08338280256676,46.0350046517945,-4.20419767461094));
#25299=CARTESIAN_POINT('Ctrl Pts',(-7.51545706022845,45.9802696389798,-5.17533847162807));
#25300=CARTESIAN_POINT('Ctrl Pts',(-7.96942443679653,45.8732160711656,-7.20182382545928));
#25301=CARTESIAN_POINT('Ctrl Pts',(-7.99777112386962,45.8238046792999,-8.23520088124158));
#25302=CARTESIAN_POINT('Ctrl Pts',(-7.65816151419308,45.7182688493223,-10.2680218936531));
#25303=CARTESIAN_POINT('Ctrl Pts',(-7.28861749067,45.6641325228415,-11.2473221839934));
#25304=CARTESIAN_POINT('Ctrl Pts',(-6.19253387136322,45.5597638414915,-13.0106480423953));
#25305=CARTESIAN_POINT('Ctrl Pts',(-5.47569444764857,45.5081470312241,-13.7771188700226));
#25306=CARTESIAN_POINT('Ctrl Pts',(-3.79990067038661,45.4013065309656,-14.9811725513299));
#25307=CARTESIAN_POINT('Ctrl Pts',(-2.86044627530179,45.3506055844234,-15.4121480385549));
#25308=CARTESIAN_POINT('Ctrl Pts',(-1.25297119627631,45.2673752063774,-15.8007416130287));
#25309=CARTESIAN_POINT('Ctrl Pts',(-0.62684741416668,45.2349563404374,-15.875));
#25310=CARTESIAN_POINT('Ctrl Pts',(-9.71445146547012E-15,45.2025000069372,
-15.875));
#25311=CARTESIAN_POINT('Ctrl Pts',(-3.73312492030209E-14,44.885,-15.875));
#25312=CARTESIAN_POINT('Ctrl Pts',(-0.932020445293405,44.9332573042782,
-15.875));
#25313=CARTESIAN_POINT('Ctrl Pts',(-1.85769971369281,44.980244432192,-15.7108256257695));
#25314=CARTESIAN_POINT('Ctrl Pts',(-3.70421023799222,45.0782119619776,-15.0332931782654));
#25315=CARTESIAN_POINT('Ctrl Pts',(-4.59539439428895,45.1320341721975,-14.4914022865744));
#25316=CARTESIAN_POINT('Ctrl Pts',(-6.11480378672683,45.2379825132159,-13.1014187072022));
#25317=CARTESIAN_POINT('Ctrl Pts',(-6.73046087154675,45.2874149370191,-12.2685259637988));
#25318=CARTESIAN_POINT('Ctrl Pts',(-7.62026450762139,45.3939505954988,-10.3941698289853));
#25319=CARTESIAN_POINT('Ctrl Pts',(-7.87784267286048,45.4486539057136,-9.36697561457017));
#25320=CARTESIAN_POINT('Ctrl Pts',(-7.97764310122838,45.5522679542267,-7.29526241641956));
#25321=CARTESIAN_POINT('Ctrl Pts',(-7.82806540607513,45.6038084711587,-6.27111851809931));
#25322=CARTESIAN_POINT('Ctrl Pts',(-7.1443428831817,45.7104692171442,-4.32726235844925));
#25323=CARTESIAN_POINT('Ctrl Pts',(-6.61314452286045,45.7612471334107,-3.42731431463647));
#25324=CARTESIAN_POINT('Ctrl Pts',(-5.2322356449816,45.8662204115536,-1.87873993665991));
#25325=CARTESIAN_POINT('Ctrl Pts',(-4.39451134392497,45.9205611496417,-1.24622997719547));
#25326=CARTESIAN_POINT('Ctrl Pts',(-2.53754931859762,46.0257066178352,-0.347228690382674));
#25327=CARTESIAN_POINT('Ctrl Pts',(-1.53878048653146,46.07532642789,-0.0836158856518243));
#25328=CARTESIAN_POINT('Ctrl Pts',(0.530475862045332,46.1824664951999,0.0515848033244231));
#25329=CARTESIAN_POINT('Ctrl Pts',(1.58161651110608,46.2363802475909,-0.0886182285104546));
#25330=CARTESIAN_POINT('Ctrl Pts',(3.55013587705037,46.3393838294781,-0.763695491740995));
#25331=CARTESIAN_POINT('Ctrl Pts',(4.4509168543477,46.3929808139443,-1.28497698088934));
#25332=CARTESIAN_POINT('Ctrl Pts',(6.0003125392266,46.4991411338195,-2.6406532119956));
#25333=CARTESIAN_POINT('Ctrl Pts',(6.63505294201067,46.5487392394636,-3.46129238829061));
#25334=CARTESIAN_POINT('Ctrl Pts',(7.56467089723176,46.6549223179508,-5.31555205511408));
#25335=CARTESIAN_POINT('Ctrl Pts',(7.84407828082769,46.7095721457825,-6.33456743405312));
#25336=CARTESIAN_POINT('Ctrl Pts',(7.98993006677436,46.8136199865895,-8.40012686786143));
#25337=CARTESIAN_POINT('Ctrl Pts',(7.8636353537285,46.8644913094592,-9.42623077416332));
#25338=CARTESIAN_POINT('Ctrl Pts',(7.22812604754061,46.9705556607606,-11.3736410838175));
#25339=CARTESIAN_POINT('Ctrl Pts',(6.72492600108043,47.0213593418421,-12.2766447124189));
#25340=CARTESIAN_POINT('Ctrl Pts',(5.38905941843051,47.125454127982,-13.8583488300923));
#25341=CARTESIAN_POINT('Ctrl Pts',(4.56262965766865,47.1800963018128,-14.5163090248842));
#25342=CARTESIAN_POINT('Ctrl Pts',(2.71837576444638,47.2862378264649,-15.4655301718279));
#25343=CARTESIAN_POINT('Ctrl Pts',(1.72157316290845,47.3358619554654,-15.7539546713386));
#25344=CARTESIAN_POINT('Ctrl Pts',(0.465187531251854,47.4009139444253,-15.8647882769727));
#25345=CARTESIAN_POINT('Ctrl Pts',(0.232461311524967,47.4129638303003,-15.875));
#25346=CARTESIAN_POINT('Ctrl Pts',(-9.85322934354826E-15,47.425,-15.875));
#25347=CARTESIAN_POINT('Origin',(0.,-18.001,-7.93750000000004));
#25348=CARTESIAN_POINT('',(-2.25170198433171E-14,50.2825000069373,-15.875));
#25349=CARTESIAN_POINT('',(1.77632592688644E-14,49.965,-15.875));
#25350=CARTESIAN_POINT('',(-9.72063396823211E-16,-18.001,-15.875));
#25351=CARTESIAN_POINT('Ctrl Pts',(-5.81479309147426E-14,50.2825000069373,
-15.875));
#25352=CARTESIAN_POINT('Ctrl Pts',(0.653807280817845,50.2486477700587,-15.875));
#25353=CARTESIAN_POINT('Ctrl Pts',(1.30663150140665,50.2148464331757,-15.7942160326749));
#25354=CARTESIAN_POINT('Ctrl Pts',(2.9366542847825,50.1304486006657,-15.38259096553));
#25355=CARTESIAN_POINT('Ctrl Pts',(3.87202354333085,50.0794754540483,-14.9418443569599));
#25356=CARTESIAN_POINT('Ctrl Pts',(5.53435991943361,49.9726957425407,-13.7212655606029));
#25357=CARTESIAN_POINT('Ctrl Pts',(6.24238641304659,49.9213955529466,-12.9488528088023));
#25358=CARTESIAN_POINT('Ctrl Pts',(7.32098116949546,49.816809543527,-11.1754310887501));
#25359=CARTESIAN_POINT('Ctrl Pts',(7.68115940712471,49.7625967825885,-10.1915354788068));
#25360=CARTESIAN_POINT('Ctrl Pts',(8.00031667494626,49.6571917112352,-8.15472447597427));
#25361=CARTESIAN_POINT('Ctrl Pts',(7.96161114636959,49.6077302366269,-7.12204195811604));
#25362=CARTESIAN_POINT('Ctrl Pts',(7.48729083246518,49.500544002672,-5.09947555936591));
#25363=CARTESIAN_POINT('Ctrl Pts',(7.04489407564157,49.4458127135795,-4.13176436505925));
#25364=CARTESIAN_POINT('Ctrl Pts',(5.82244293327038,49.3432169360504,-2.44550101455162));
#25365=CARTESIAN_POINT('Ctrl Pts',(5.06205045206097,49.2898545540075,-1.73757352754138));
#25366=CARTESIAN_POINT('Ctrl Pts',(3.3130744950487,49.1835361040814,-0.651400106710352));
#25367=CARTESIAN_POINT('Ctrl Pts',(2.34118543823385,49.1337197705541,-0.283572948588524));
#25368=CARTESIAN_POINT('Ctrl Pts',(0.296287131399293,49.0278408917062,0.0629522337464999));
#25369=CARTESIAN_POINT('Ctrl Pts',(-0.75800313893461,48.9732528119812,0.0324758551607617));
#25370=CARTESIAN_POINT('Ctrl Pts',(-2.77383231753296,48.8688790479336,-0.43032492871163));
#25371=CARTESIAN_POINT('Ctrl Pts',(-3.71788481900124,48.8184553700188,-0.850245570831606));
#25372=CARTESIAN_POINT('Ctrl Pts',(-5.40884456344841,48.7115493990853,-2.03557633726835));
#25373=CARTESIAN_POINT('Ctrl Pts',(-6.1356304108929,48.6595469669848,-2.79529963316335));
#25374=CARTESIAN_POINT('Ctrl Pts',(-7.25134190837716,48.5554299408883,-4.54713752306414));
#25375=CARTESIAN_POINT('Ctrl Pts',(-7.63136315832352,48.5013858118147,-5.52116125907929));
#25376=CARTESIAN_POINT('Ctrl Pts',(-7.99395463249854,48.3957106443432,-7.54934460457188));
#25377=CARTESIAN_POINT('Ctrl Pts',(-7.9772594876316,48.3463261487214,-8.58348117451226));
#25378=CARTESIAN_POINT('Ctrl Pts',(-7.54614137792062,48.2394286218675,-10.6142219063534));
#25379=CARTESIAN_POINT('Ctrl Pts',(-7.12567396603874,48.1846960942229,-11.5890835286308));
#25380=CARTESIAN_POINT('Ctrl Pts',(-5.94309054125989,48.0816064135481,-13.2983306145831));
#25381=CARTESIAN_POINT('Ctrl Pts',(-5.20022189354574,48.0291659070723,-14.0216488963176));
#25382=CARTESIAN_POINT('Ctrl Pts',(-3.47613061226199,47.922679825768,-15.1475811993493));
#25383=CARTESIAN_POINT('Ctrl Pts',(-2.51035411875744,47.8724788321516,-15.5379545432278));
#25384=CARTESIAN_POINT('Ctrl Pts',(-1.00241195566267,47.794401978617,-15.8275351151833));
#25385=CARTESIAN_POINT('Ctrl Pts',(-0.501168007523581,47.7684490267852,
-15.875));
#25386=CARTESIAN_POINT('Ctrl Pts',(2.04003480774873E-14,47.7425000069373,
-15.875));
#25387=CARTESIAN_POINT('Ctrl Pts',(-1.56819002228303E-14,47.425,-15.875));
#25388=CARTESIAN_POINT('Ctrl Pts',(-0.794856362164506,47.466155347525,-15.875));
#25389=CARTESIAN_POINT('Ctrl Pts',(-1.58661550937941,47.5071503302801,-15.7555961361419));
#25390=CARTESIAN_POINT('Ctrl Pts',(-3.35195554599498,47.5985544960704,-15.2088091003677));
#25391=CARTESIAN_POINT('Ctrl Pts',(-4.28395883803311,47.652585540312,-14.701794946948));
#25392=CARTESIAN_POINT('Ctrl Pts',(-5.87552731412188,47.7597364624359,-13.3716151818296));
#25393=CARTESIAN_POINT('Ctrl Pts',(-6.52653109150684,47.8093289243409,-12.5695465207045));
#25394=CARTESIAN_POINT('Ctrl Pts',(-7.4955427314391,47.9145121408912,-10.7483913152514));
#25395=CARTESIAN_POINT('Ctrl Pts',(-7.79883064150281,47.9688360087522,-9.74375461563591));
#25396=CARTESIAN_POINT('Ctrl Pts',(-8.00057468876214,48.0737561993779,-7.67864045101106));
#25397=CARTESIAN_POINT('Ctrl Pts',(-7.8986131005827,48.1246022992544,-6.63822515393834));
#25398=CARTESIAN_POINT('Ctrl Pts',(-7.30387333168754,48.2312802090904,-4.66510819031687));
#25399=CARTESIAN_POINT('Ctrl Pts',(-6.82057134758887,48.282736323223,-3.75004758489364));
#25400=CARTESIAN_POINT('Ctrl Pts',(-5.51816506889115,48.386402537996,-2.13637139113658));
#25401=CARTESIAN_POINT('Ctrl Pts',(-4.70449046280344,48.4411009476239,-1.45900742530222));
#25402=CARTESIAN_POINT('Ctrl Pts',(-2.8805040993486,48.5475969906744,-0.47024158232038));
#25403=CARTESIAN_POINT('Ctrl Pts',(-1.89190398115398,48.5970427217612,-0.160743512346776));
#25404=CARTESIAN_POINT('Ctrl Pts',(0.154842771348392,48.7030173077424,0.065423053042827));
#25405=CARTESIAN_POINT('Ctrl Pts',(1.19386045451051,48.756814617383,-0.0226010476609183));
#25406=CARTESIAN_POINT('Ctrl Pts',(3.19252183340366,48.8602994827606,-0.595418601074552));
#25407=CARTESIAN_POINT('Ctrl Pts',(4.13143524810454,48.913349841068,-1.07966736250788));
#25408=CARTESIAN_POINT('Ctrl Pts',(5.74941340285591,49.0203991123348,-2.37015725975462));
#25409=CARTESIAN_POINT('Ctrl Pts',(6.41852304397825,49.070288107611,-3.15695120719297));
#25410=CARTESIAN_POINT('Ctrl Pts',(7.43015648945349,49.1751261096768,-4.95724731194615));
#25411=CARTESIAN_POINT('Ctrl Pts',(7.75674079541332,49.2295856951343,-5.95707063619724));
#25412=CARTESIAN_POINT('Ctrl Pts',(8.00398623965225,49.3349570883735,-8.01656328924397));
#25413=CARTESIAN_POINT('Ctrl Pts',(7.92584933507523,49.3852621659541,-9.05594985543086));
#25414=CARTESIAN_POINT('Ctrl Pts',(7.37745291223851,49.4917846730923,-11.0409688476393));
#25415=CARTESIAN_POINT('Ctrl Pts',(6.91454042622445,49.5440318327638,-11.9682759154278));
#25416=CARTESIAN_POINT('Ctrl Pts',(5.64664929693399,49.6472299724739,-13.6140780353494));
#25417=CARTESIAN_POINT('Ctrl Pts',(4.84639023667935,49.701959249045,-14.3109211479442));
#25418=CARTESIAN_POINT('Ctrl Pts',(3.04350605084262,49.8087869894479,-15.339630622804));
#25419=CARTESIAN_POINT('Ctrl Pts',(2.06327777697,49.858169485716,-15.6703754064018));
#25420=CARTESIAN_POINT('Ctrl Pts',(0.699355133000662,49.928789427987,-15.8519168472916));
#25421=CARTESIAN_POINT('Ctrl Pts',(0.349501826097301,49.9469038133199,-15.875));
#25422=CARTESIAN_POINT('Ctrl Pts',(2.98372437868011E-14,49.965,-15.875));
#25423=CARTESIAN_POINT('Origin',(0.,-18.001,-7.93750000000004));
#25424=CARTESIAN_POINT('',(3.23349364670696E-14,52.8225000069373,-15.875));
#25425=CARTESIAN_POINT('',(-1.58903761650857E-14,52.505,-15.875));
#25426=CARTESIAN_POINT('',(-9.72063396823211E-16,-18.001,-15.875));
#25427=CARTESIAN_POINT('Ctrl Pts',(6.45317133063372E-14,52.8225000069373,
-15.875));
#25428=CARTESIAN_POINT('Ctrl Pts',(0.773569576646692,52.7824468271716,-15.875));
#25429=CARTESIAN_POINT('Ctrl Pts',(1.54453904921656,52.7425282732227,-15.7619059751812));
#25430=CARTESIAN_POINT('Ctrl Pts',(3.27171771156026,52.6530999922527,-15.2419447488513));
#25431=CARTESIAN_POINT('Ctrl Pts',(4.18864284441362,52.6006075124872,-14.757666944871));
#25432=CARTESIAN_POINT('Ctrl Pts',(5.79044053510198,52.4941311371167,-13.463730874213));
#25433=CARTESIAN_POINT('Ctrl Pts',(6.45897797152374,52.4439565573702,-12.665085600608));
#25434=CARTESIAN_POINT('Ctrl Pts',(7.45808107910025,52.3384627919826,-10.8474012410675));
#25435=CARTESIAN_POINT('Ctrl Pts',(7.77536200962594,52.2839696599145,-9.84387381973884));
#25436=CARTESIAN_POINT('Ctrl Pts',(8.00184684110837,52.1792355660142,-7.7905775789266));
#25437=CARTESIAN_POINT('Ctrl Pts',(7.91628553375303,52.1292389925771,-6.76125855492272));
#25438=CARTESIAN_POINT('Ctrl Pts',(7.35317347218804,52.0222212289997,-4.77096355284263));
#25439=CARTESIAN_POINT('Ctrl Pts',(6.87284289780254,51.9694296557435,-3.8314173847343));
#25440=CARTESIAN_POINT('Ctrl Pts',(5.58300909250724,51.8657943866653,-2.20145348555862));
#25441=CARTESIAN_POINT('Ctrl Pts',(4.78946963612395,51.8119365510112,-1.52399560683276));
#25442=CARTESIAN_POINT('Ctrl Pts',(2.99409950398244,51.7060271422976,-0.515118645584527));
#25443=CARTESIAN_POINT('Ctrl Pts',(2.01075948761862,51.6566112771505,-0.190679533404238));
#25444=CARTESIAN_POINT('Ctrl Pts',(-0.0479242187475715,51.5500186304629,
0.0688836502428259));
#25445=CARTESIAN_POINT('Ctrl Pts',(-1.10456567771461,51.4953088130379,-0.00752102230742142));
#25446=CARTESIAN_POINT('Ctrl Pts',(-3.1042403601309,51.391771481755,-0.56054811777542));
#25447=CARTESIAN_POINT('Ctrl Pts',(-4.03048770719061,51.3401050408273,-1.02294329308526));
#25448=CARTESIAN_POINT('Ctrl Pts',(-5.66283575348142,51.2334696110068,-2.28005664868103));
#25449=CARTESIAN_POINT('Ctrl Pts',(-6.35126848200509,51.1827882120263,-3.06556267474446));
#25450=CARTESIAN_POINT('Ctrl Pts',(-7.39065099008283,51.0777381993738,-4.86114796347009));
#25451=CARTESIAN_POINT('Ctrl Pts',(-7.7297322817676,51.0233734807042,-5.85498426542378));
#25452=CARTESIAN_POINT('Ctrl Pts',(-8.00311693857964,50.9182838662122,-7.90026155689908));
#25453=CARTESIAN_POINT('Ctrl Pts',(-7.94125568753201,50.868621142215,-8.93132691420704));
#25454=CARTESIAN_POINT('Ctrl Pts',(-7.42295486627348,50.7614972641422,-10.9383368889781));
#25455=CARTESIAN_POINT('Ctrl Pts',(-6.96162877025295,50.7077522190565,-11.8923214807642));
#25456=CARTESIAN_POINT('Ctrl Pts',(-5.7056586211759,50.604656784673,-13.5511567107216));
#25457=CARTESIAN_POINT('Ctrl Pts',(-4.92875937155118,50.5510208328049,-14.2442271685858));
#25458=CARTESIAN_POINT('Ctrl Pts',(-3.15674152402518,50.4448934073684,-15.2924094280659));
#25459=CARTESIAN_POINT('Ctrl Pts',(-2.17916238406381,50.3953306886788,-15.6388624867812));
#25460=CARTESIAN_POINT('Ctrl Pts',(-0.776895600253733,50.3227253985187,
-15.8465111808394));
#25461=CARTESIAN_POINT('Ctrl Pts',(-0.388274448369631,50.3026037270789,
-15.875));
#25462=CARTESIAN_POINT('Ctrl Pts',(-6.26582119522823E-14,50.2825000069373,
-15.875));
#25463=CARTESIAN_POINT('Ctrl Pts',(2.23432383705813E-14,49.965,-15.875));
#25464=CARTESIAN_POINT('Ctrl Pts',(-0.681261075343724,50.0002737144038,
-15.875));
#25465=CARTESIAN_POINT('Ctrl Pts',(-1.361186693817,50.03547828274,-15.7872884588347));
#25466=CARTESIAN_POINT('Ctrl Pts',(-3.03049655359253,50.121910285648,-15.3473599347427));
#25467=CARTESIAN_POINT('Ctrl Pts',(-3.97616063868438,50.1740893961102,-14.885896974024));
#25468=CARTESIAN_POINT('Ctrl Pts',(-5.62029138243705,50.2810227358729,-13.6352123273661));
#25469=CARTESIAN_POINT('Ctrl Pts',(-6.30743060757244,50.3313360092099,-12.8637472404363));
#25470=CARTESIAN_POINT('Ctrl Pts',(-7.36127462030046,50.4357969462637,-11.0848234209427));
#25471=CARTESIAN_POINT('Ctrl Pts',(-7.71098839802158,50.4903648478974,-10.0903156889372));
#25472=CARTESIAN_POINT('Ctrl Pts',(-8.00342981178138,50.5961556729552,-8.03699049288612));
#25473=CARTESIAN_POINT('Ctrl Pts',(-7.94880387175336,50.6460463980019,-6.99874079620579));
#25474=CARTESIAN_POINT('Ctrl Pts',(-7.44623828915304,50.7524027784839,-5.00220407522544));
#25475=CARTESIAN_POINT('Ctrl Pts',(-7.00351678260699,50.8055523242616,-4.06287997598149));
#25476=CARTESIAN_POINT('Ctrl Pts',(-5.77000092114518,50.9082591534721,-2.38590793487282));
#25477=CARTESIAN_POINT('Ctrl Pts',(-4.98334557363517,50.9629928732215,-1.67019492318765));
#25478=CARTESIAN_POINT('Ctrl Pts',(-3.20166662664349,51.0701180942583,-0.602524264433342));
#25479=CARTESIAN_POINT('Ctrl Pts',(-2.22968898315318,51.1195531981091,-0.251080012551294));
#25480=CARTESIAN_POINT('Ctrl Pts',(-0.192751057308643,51.2250199116128,
0.0651712897973573));
#25481=CARTESIAN_POINT('Ctrl Pts',(0.853616143887715,51.2791977578927,0.0218546860159068));
#25482=CARTESIAN_POINT('Ctrl Pts',(2.87160605675112,51.3836833984677,-0.465122895034999));
#25483=CARTESIAN_POINT('Ctrl Pts',(3.82364940164646,51.4351278390047,-0.904556148837716));
#25484=CARTESIAN_POINT('Ctrl Pts',(5.49281377843064,51.5419361314569,-2.11667612674403));
#25485=CARTESIAN_POINT('Ctrl Pts',(6.19730349890426,51.5927796532965,-2.87327719099847));
#25486=CARTESIAN_POINT('Ctrl Pts',(7.29152515539215,51.696846704379,-4.63108268685891));
#25487=CARTESIAN_POINT('Ctrl Pts',(7.66340527550933,51.7514934477553,-5.61998921481477));
#25488=CARTESIAN_POINT('Ctrl Pts',(7.99920554623815,51.8576596089564,-7.66684839583198));
#25489=CARTESIAN_POINT('Ctrl Pts',(7.96700279068472,51.9072681563388,-8.70390841509103));
#25490=CARTESIAN_POINT('Ctrl Pts',(7.50831207286596,52.013437504532,-10.7109027891529));
#25491=CARTESIAN_POINT('Ctrl Pts',(7.08505449358577,52.0670234901091,-11.6615744498179));
#25492=CARTESIAN_POINT('Ctrl Pts',(5.88754951617242,52.170001284794,-13.3637011068002));
#25493=CARTESIAN_POINT('Ctrl Pts',(5.11866135152908,52.223962717717,-14.0943366610575));
#25494=CARTESIAN_POINT('Ctrl Pts',(3.36375569476365,52.3311072364392,-15.1994916795358));
#25495=CARTESIAN_POINT('Ctrl Pts',(2.40037277456299,52.3807156884826,-15.5722639209813));
#25496=CARTESIAN_POINT('Ctrl Pts',(0.931959596462894,52.4567458462968,-15.833983701258));
#25497=CARTESIAN_POINT('Ctrl Pts',(0.465883173992151,52.4808779260702,-15.875));
#25498=CARTESIAN_POINT('Ctrl Pts',(-3.24740234702858E-14,52.505,-15.875));
#25499=CARTESIAN_POINT('Origin',(0.,-18.001,-7.93750000000004));
#25500=CARTESIAN_POINT('',(-2.46333824840088E-14,55.3625000069373,-15.875));
#25501=CARTESIAN_POINT('',(2.44592918861349E-14,55.045,-15.875));
#25502=CARTESIAN_POINT('',(-9.72063396823211E-16,-18.001,-15.875));
#25503=CARTESIAN_POINT('Ctrl Pts',(-2.52575738102223E-14,55.3625000069373,
-15.875));
#25504=CARTESIAN_POINT('Ctrl Pts',(0.88761857172687,55.3165417023581,-15.875));
#25505=CARTESIAN_POINT('Ctrl Pts',(1.77011756769855,55.2713889565383,-15.7260946063877));
#25506=CARTESIAN_POINT('Ctrl Pts',(3.58449937240897,55.1761581973968,-15.0942661122647));
#25507=CARTESIAN_POINT('Ctrl Pts',(4.48318907247908,55.1225090905112,-14.5683935783575));
#25508=CARTESIAN_POINT('Ctrl Pts',(6.02596616795313,55.0163930988054,-13.2050641840642));
#25509=CARTESIAN_POINT('Ctrl Pts',(6.65647325827018,54.9668417440083,-12.3816969617684));
#25510=CARTESIAN_POINT('Ctrl Pts',(7.57729478212815,54.8605781437163,-10.5229439661176));
#25511=CARTESIAN_POINT('Ctrl Pts',(7.85188655635563,54.8059142458295,-9.50207817347011));
#25512=CARTESIAN_POINT('Ctrl Pts',(7.98755464789972,54.7019597341018,-7.43510513527449));
#25513=CARTESIAN_POINT('Ctrl Pts',(7.85611325111853,54.6509510053513,-6.40942676133224));
#25514=CARTESIAN_POINT('Ctrl Pts',(7.20649584389212,54.5441790337993,-4.45223046677657));
#25515=CARTESIAN_POINT('Ctrl Pts',(6.68964065097011,54.4929165656096,-3.54098331751992));
#25516=CARTESIAN_POINT('Ctrl Pts',(5.33445751776623,54.3883039015244,-1.96884961653697));
#25517=CARTESIAN_POINT('Ctrl Pts',(4.50911833992717,54.3340819831997,-1.32319720029189));
#25518=CARTESIAN_POINT('Ctrl Pts',(2.66936874471942,54.2286936544334,-0.392525075909464));
#25519=CARTESIAN_POINT('Ctrl Pts',(1.67495331423129,54.1792242114812,-0.111474355579484));
#25520=CARTESIAN_POINT('Ctrl Pts',(-0.395625268275944,54.0720156827491,
0.0598698134383127));
#25521=CARTESIAN_POINT('Ctrl Pts',(-1.45258479174199,54.017296838446,-0.0632474876637047));
#25522=CARTESIAN_POINT('Ctrl Pts',(-3.43343402764324,53.9147195090952,-0.707348252054608));
#25523=CARTESIAN_POINT('Ctrl Pts',(-4.34111091272081,53.861307471052,-1.21306133286519));
#25524=CARTESIAN_POINT('Ctrl Pts',(-5.91269534406702,53.755009034774,-2.54273563012737));
#25525=CARTESIAN_POINT('Ctrl Pts',(-6.56172013952658,53.7052112496336,-3.35412661619982));
#25526=CARTESIAN_POINT('Ctrl Pts',(-7.52086783897476,53.5993094898124,-5.19307861402896));
#25527=CARTESIAN_POINT('Ctrl Pts',(-7.81640836407917,53.5447163268471,-6.20570129682935));
#25528=CARTESIAN_POINT('Ctrl Pts',(-7.99648604030202,53.4403657138208,-8.26628860586363));
#25529=CARTESIAN_POINT('Ctrl Pts',(-7.88748313012729,53.3899120148144,-9.29379040068007));
#25530=CARTESIAN_POINT('Ctrl Pts',(-7.28013210091988,53.2830133436423,-11.2672928240728));
#25531=CARTESIAN_POINT('Ctrl Pts',(-6.78109645907326,53.2310564179884,-12.1924339505509));
#25532=CARTESIAN_POINT('Ctrl Pts',(-5.45783190275612,53.1269103387079,-13.7931686694191));
#25533=CARTESIAN_POINT('Ctrl Pts',(-4.64796834669153,53.0728553747377,-14.4546356330282));
#25534=CARTESIAN_POINT('Ctrl Pts',(-2.82977960591002,52.9671956648927,-15.4239008199022));
#25535=CARTESIAN_POINT('Ctrl Pts',(-1.84076920880454,52.9178096755865,-15.7262998319337));
#25536=CARTESIAN_POINT('Ctrl Pts',(-0.54814992503158,52.8508816136455,-15.8608219119256));
#25537=CARTESIAN_POINT('Ctrl Pts',(-0.273911963877,52.8366823706966,-15.875));
#25538=CARTESIAN_POINT('Ctrl Pts',(6.85562717706034E-14,52.8225000069373,
-15.875));
#25539=CARTESIAN_POINT('Ctrl Pts',(-3.42781358853017E-14,52.505,-15.875));
#25540=CARTESIAN_POINT('Ctrl Pts',(-0.568805192377397,52.5344510762958,
-15.875));
#25541=CARTESIAN_POINT('Ctrl Pts',(-1.13732232065543,52.5638872374713,-15.8138577872502));
#25542=CARTESIAN_POINT('Ctrl Pts',(-2.70703094247271,52.6451621783525,-15.4706097604538));
#25543=CARTESIAN_POINT('Ctrl Pts',(-3.66545458389885,52.6959677070125,-15.0536927628113));
#25544=CARTESIAN_POINT('Ctrl Pts',(-5.35996431105652,52.8026354726181,-13.8810751253922));
#25545=CARTESIAN_POINT('Ctrl Pts',(-6.08211127948475,52.8541413740709,-13.139716279437));
#25546=CARTESIAN_POINT('Ctrl Pts',(-7.21715707056025,52.9577767420853,-11.4039417446916));
#25547=CARTESIAN_POINT('Ctrl Pts',(-7.61147670373317,53.0124780967622,-10.4212172385492));
#25548=CARTESIAN_POINT('Ctrl Pts',(-7.99124082629523,53.1189976509299,-8.38146625795112));
#25549=CARTESIAN_POINT('Ctrl Pts',(-7.98165426017353,53.1684353096838,-7.3457038996455));
#25550=CARTESIAN_POINT('Ctrl Pts',(-7.56733219350833,53.274394399366,-5.32856309764741));
#25551=CARTESIAN_POINT('Ctrl Pts',(-7.16391753611599,53.3282065003057,-4.36685224739507));
#25552=CARTESIAN_POINT('Ctrl Pts',(-6.00411927873589,53.4317278818505,-2.64143505455244));
#25553=CARTESIAN_POINT('Ctrl Pts',(-5.2547732797613,53.4847149013944,-1.89718788925229));
#25554=CARTESIAN_POINT('Ctrl Pts',(-3.52949948587456,53.5917566649436,-0.754624459901292));
#25555=CARTESIAN_POINT('Ctrl Pts',(-2.57506355292129,53.6416707087415,-0.359892258863898));
#25556=CARTESIAN_POINT('Ctrl Pts',(-0.550748628270484,53.746483840006,0.0491226757877679));
#25557=CARTESIAN_POINT('Ctrl Pts',(0.501220410293203,53.8009517331103,0.0523834362455195));
#25558=CARTESIAN_POINT('Ctrl Pts',(2.53689294035174,53.9063529281055,-0.345805101373066));
#25559=CARTESIAN_POINT('Ctrl Pts',(3.50169336609131,53.9566255404585,-0.739738490901493));
#25560=CARTESIAN_POINT('Ctrl Pts',(5.22183529061327,54.0631369800951,-1.87193984619186));
#25561=CARTESIAN_POINT('Ctrl Pts',(5.96193048657355,54.1154425953717,-2.59768254400995));
#25562=CARTESIAN_POINT('Ctrl Pts',(7.13817560015142,54.2186077349236,-4.31052145182514));
#25563=CARTESIAN_POINT('Ctrl Pts',(7.55515623808315,54.2733381452226,-5.28647299768086));
#25564=CARTESIAN_POINT('Ctrl Pts',(7.97941717874886,54.3801873812773,-7.31846109431562));
#25565=CARTESIAN_POINT('Ctrl Pts',(7.99261080995647,54.4295698712085,-8.35282137566351));
#25566=CARTESIAN_POINT('Ctrl Pts',(7.6231181130602,54.5352853019203,-10.379580022952));
#25567=CARTESIAN_POINT('Ctrl Pts',(7.2399605875748,54.5893004394446,-11.3519959759335));
#25568=CARTESIAN_POINT('Ctrl Pts',(6.1183600267905,54.6933403475528,-13.1003543210902));
#25569=CARTESIAN_POINT('Ctrl Pts',(5.38857828921182,54.7454647732774,-13.8580363977351));
#25570=CARTESIAN_POINT('Ctrl Pts',(3.69305506784267,54.8523898023613,-15.0377122934536));
#25571=CARTESIAN_POINT('Ctrl Pts',(2.74762010323095,54.9027362331134,-15.454297360553));
#25572=CARTESIAN_POINT('Ctrl Pts',(1.17380103557826,54.9842240009087,-15.8098607310094));
#25573=CARTESIAN_POINT('Ctrl Pts',(0.587101634914653,55.0146015871955,-15.875));
#25574=CARTESIAN_POINT('Ctrl Pts',(6.80011602582908E-14,55.045,-15.875));
#25575=CARTESIAN_POINT('Origin',(0.,-18.001,-7.93750000000004));
#25576=CARTESIAN_POINT('',(-1.94292120560783E-14,57.9025000069372,-15.875));
#25577=CARTESIAN_POINT('',(8.2569746205115E-15,57.585,-15.875));
#25578=CARTESIAN_POINT('',(-9.72063396823211E-16,-18.001,-15.875));
#25579=CARTESIAN_POINT('Ctrl Pts',(-1.94289029309402E-14,57.9025000069372,
-15.875));
#25580=CARTESIAN_POINT('Ctrl Pts',(1.00230603299107,57.8506035196249,-15.875));
#25581=CARTESIAN_POINT('Ctrl Pts',(1.9959609410133,57.8006823389778,-15.6851412199518));
#25582=CARTESIAN_POINT('Ctrl Pts',(3.89102299059962,57.6984103445198,-14.9329972766124));
#25583=CARTESIAN_POINT('Ctrl Pts',(4.76979217675884,57.6443450358377,-14.3660308679274));
#25584=CARTESIAN_POINT('Ctrl Pts',(6.25173435119394,57.5387003001706,-12.9344540107633));
#25585=CARTESIAN_POINT('Ctrl Pts',(6.84387225904376,57.4893124928267,-12.086611652602));
#25586=CARTESIAN_POINT('Ctrl Pts',(7.68405028232776,57.3823794642433,-10.1880615929251));
#25587=CARTESIAN_POINT('Ctrl Pts',(7.91431425195137,57.3276457713469,-9.15137546263761));
#25588=CARTESIAN_POINT('Ctrl Pts',(7.95686252569159,57.2246127701732,-7.07285951960697));
#25589=CARTESIAN_POINT('Ctrl Pts',(7.77829154751339,57.1720698458426,-6.05128377736823));
#25590=CARTESIAN_POINT('Ctrl Pts',(7.04015426818784,57.0656028579094,-4.12904278181492));
#25591=CARTESIAN_POINT('Ctrl Pts',(6.48613432213068,57.0154533099021,-3.2472746964605));
#25592=CARTESIAN_POINT('Ctrl Pts',(5.06426424004539,56.9099352259738,-1.7371772449326));
#25593=CARTESIAN_POINT('Ctrl Pts',(4.2070022646224,56.8554356091949,-1.12633812031294));
#25594=CARTESIAN_POINT('Ctrl Pts',(2.32294817932973,56.7507227367625,-0.278840170685674));
#25595=CARTESIAN_POINT('Ctrl Pts',(1.31724792115926,56.7007032679948,-0.0434516304225713));
#25596=CARTESIAN_POINT('Ctrl Pts',(-0.749521171617977,56.5936919835465,
0.0333113444225467));
#25597=CARTESIAN_POINT('Ctrl Pts',(-1.7910609478416,56.5409514172919,-0.134456053490981));
#25598=CARTESIAN_POINT('Ctrl Pts',(-3.73884162559752,56.4372861119748,-0.85982070936449));
#25599=CARTESIAN_POINT('Ctrl Pts',(-4.62778972832387,56.3834163166858,-1.40635282421876));
#25600=CARTESIAN_POINT('Ctrl Pts',(-6.14034710128368,56.2775203576562,-2.80404622174758));
#25601=CARTESIAN_POINT('Ctrl Pts',(-6.75167720510281,56.2281093692751,-3.63970193484849));
#25602=CARTESIAN_POINT('Ctrl Pts',(-7.6323961671839,56.1214975064136,-5.51855737820616));
#25603=CARTESIAN_POINT('Ctrl Pts',(-7.88498224369959,56.066785643353,-6.54754730732683));
#25604=CARTESIAN_POINT('Ctrl Pts',(-7.97428981649316,55.9632746391773,-8.6205772700019));
#25605=CARTESIAN_POINT('Ctrl Pts',(-7.81940301583157,55.9115645027195,-9.64426158415518));
#25606=CARTESIAN_POINT('Ctrl Pts',(-7.12570651529608,55.8049377806125,-11.584186062756));
#25607=CARTESIAN_POINT('Ctrl Pts',(-6.59031936774201,55.7542884945185,-12.4808155020628));
#25608=CARTESIAN_POINT('Ctrl Pts',(-5.20189381553948,55.6492125077333,-14.0224188859396));
#25609=CARTESIAN_POINT('Ctrl Pts',(-4.36056678196882,55.5948397826011,-14.6510211460246));
#25610=CARTESIAN_POINT('Ctrl Pts',(-2.49860396205691,55.4897694274817,-15.5406713495898));
#25611=CARTESIAN_POINT('Ctrl Pts',(-1.49856329833446,55.4400912501693,-15.7991481118117));
#25612=CARTESIAN_POINT('Ctrl Pts',(-0.318002086543258,55.378965228842,-15.8702274642353));
#25613=CARTESIAN_POINT('Ctrl Pts',(-0.158918541145936,55.3707283461698,
-15.875));
#25614=CARTESIAN_POINT('Ctrl Pts',(-4.04537514597791E-14,55.3625000069373,
-15.875));
#25615=CARTESIAN_POINT('Ctrl Pts',(6.75848266240564E-14,55.045,-15.875));
#25616=CARTESIAN_POINT('Ctrl Pts',(-0.452205833663068,55.0684139010809,
-15.875));
#25617=CARTESIAN_POINT('Ctrl Pts',(-0.904650297188487,55.0918401577207,
-15.836356781565));
#25618=CARTESIAN_POINT('Ctrl Pts',(-2.36712438493148,55.1675628067331,-15.5834915453526));
#25619=CARTESIAN_POINT('Ctrl Pts',(-3.33808801962979,55.2174301128519,-15.212223217014));
#25620=CARTESIAN_POINT('Ctrl Pts',(-5.08327993400997,55.3237749298375,-14.1199751343461));
#25621=CARTESIAN_POINT('Ctrl Pts',(-5.84100233549749,55.3769891161994,-13.4096943856778));
#25622=CARTESIAN_POINT('Ctrl Pts',(-7.0573993431594,55.4796620485725,-11.7198971070282));
#25623=CARTESIAN_POINT('Ctrl Pts',(-7.49646653809424,55.5343951520355,-10.7510672271912));
#25624=CARTESIAN_POINT('Ctrl Pts',(-7.96421846051841,55.6415392240897,-8.72722283067459));
#25625=CARTESIAN_POINT('Ctrl Pts',(-7.99958288630385,55.6909818503537,-7.69431432987161));
#25626=CARTESIAN_POINT('Ctrl Pts',(-7.67382709560291,55.7964298005714,-5.65877655536126));
#25627=CARTESIAN_POINT('Ctrl Pts',(-7.31062296358912,55.8506184786743,-4.6763531798273));
#25628=CARTESIAN_POINT('Ctrl Pts',(-6.22638360369634,55.9551350507709,-2.90617559972928));
#25629=CARTESIAN_POINT('Ctrl Pts',(-5.51551775745132,56.0065346684165,-2.13567353567475));
#25630=CARTESIAN_POINT('Ctrl Pts',(-3.84884362045724,56.113334246933,-0.920412360942083));
#25631=CARTESIAN_POINT('Ctrl Pts',(-2.91215705111828,56.1642169891423,-0.482811428301656));
#25632=CARTESIAN_POINT('Ctrl Pts',(-0.902774366284792,56.2682569725173,
0.0176270306812168));
#25633=CARTESIAN_POINT('Ctrl Pts',(0.152732482785965,56.3229080431463,0.0672248201678767));
#25634=CARTESIAN_POINT('Ctrl Pts',(2.20363894720756,56.4290980068961,-0.243069237349244));
#25635=CARTESIAN_POINT('Ctrl Pts',(3.18036814836036,56.4786919234767,-0.592738436171752));
#25636=CARTESIAN_POINT('Ctrl Pts',(4.9489277748518,56.5848485409494,-1.64663972616407));
#25637=CARTESIAN_POINT('Ctrl Pts',(5.72336896610363,56.6384499971866,-2.34195994698209));
#25638=CARTESIAN_POINT('Ctrl Pts',(6.97435306189161,56.7414640804755,-4.0049848404559));
#25639=CARTESIAN_POINT('Ctrl Pts',(7.43287526798715,56.7953584552385,-4.96108228034264));
#25640=CARTESIAN_POINT('Ctrl Pts',(7.94457635178483,56.9024966980779,-6.97052835202683));
#25641=CARTESIAN_POINT('Ctrl Pts',(8.0029508044703,56.9521212196272,-8.00184288282747));
#25642=CARTESIAN_POINT('Ctrl Pts',(7.72266974891675,57.0572603672783,-10.0458852922068));
#25643=CARTESIAN_POINT('Ctrl Pts',(7.38039817878971,57.1116038770423,-11.0382543104064));
#25644=CARTESIAN_POINT('Ctrl Pts',(6.33510138818855,57.2165859458937,-12.8305381647968));
#25645=CARTESIAN_POINT('Ctrl Pts',(5.6437278518194,57.2673526819247,-13.6140890221231));
#25646=CARTESIAN_POINT('Ctrl Pts',(4.00687273557042,57.3740105583108,-14.8657364817318));
#25647=CARTESIAN_POINT('Ctrl Pts',(3.07925268208924,57.4255652640134,-15.3248888283259));
#25648=CARTESIAN_POINT('Ctrl Pts',(1.40746958896367,57.5121253237411,-15.7811964611633));
#25649=CARTESIAN_POINT('Ctrl Pts',(0.704519872836865,57.5485220128,-15.875));
#25650=CARTESIAN_POINT('Ctrl Pts',(4.53803661315533E-14,57.585,-15.875));
#25651=CARTESIAN_POINT('Origin',(0.,-18.001,-7.93750000000004));
#25652=CARTESIAN_POINT('',(-2.07476018978207E-14,60.4425000069372,-15.875));
#25653=CARTESIAN_POINT('',(-6.10653576057646E-15,60.125,-15.875));
#25654=CARTESIAN_POINT('',(-9.72063396823211E-16,-18.001,-15.875));
#25655=CARTESIAN_POINT('Ctrl Pts',(-3.1866062751E-14,60.4425000069372,-15.875));
#25656=CARTESIAN_POINT('Ctrl Pts',(0.0810659007883464,60.4383026506875,
-15.875));
#25657=CARTESIAN_POINT('Ctrl Pts',(0.162182741164532,60.4341026569347,-15.8737581149016));
#25658=CARTESIAN_POINT('Ctrl Pts',(1.27711240176256,60.3763748461854,-15.8395640913277));
#25659=CARTESIAN_POINT('Ctrl Pts',(2.29479964502656,60.3257591259032,-15.6061075714052));
#25660=CARTESIAN_POINT('Ctrl Pts',(4.18883445623646,60.2206557380066,-14.7595152794035));
#25661=CARTESIAN_POINT('Ctrl Pts',(5.04594995342874,60.166274628506,-14.1523684799919));
#25662=CARTESIAN_POINT('Ctrl Pts',(6.4654526326233,60.0612247880728,-12.654398213762));
#25663=CARTESIAN_POINT('Ctrl Pts',(7.01909774746457,60.0115297902125,-11.7824239693426));
#25664=CARTESIAN_POINT('Ctrl Pts',(7.77410531512426,59.9044175293509,-9.85256059500888));
#25665=CARTESIAN_POINT('Ctrl Pts',(7.95883998364154,59.8507892297312,-8.8096612890105));
#25666=CARTESIAN_POINT('Ctrl Pts',(7.91262212587057,59.7476296544674,-6.72976726518009));
#25667=CARTESIAN_POINT('Ctrl Pts',(7.68884565251932,59.6939666898923,-5.71271701463284));
#25668=CARTESIAN_POINT('Ctrl Pts',(6.86647297847103,59.5878629275397,-3.82522195452598));
#25669=CARTESIAN_POINT('Ctrl Pts',(6.27718915538661,59.5383232157608,-2.97199908110532));
#25670=CARTESIAN_POINT('Ctrl Pts',(4.7920745275957,59.4320381060541,-1.52374719664043));
#25671=CARTESIAN_POINT('Ctrl Pts',(3.90515282460579,59.3773706251354,-0.948215472250059));
#25672=CARTESIAN_POINT('Ctrl Pts',(1.98005962899069,59.2734415871574,-0.182958397065402));
#25673=CARTESIAN_POINT('Ctrl Pts',(0.96364416930764,59.2223946955456,0.00762683433684866));
#25674=CARTESIAN_POINT('Ctrl Pts',(-1.09834352675043,59.1156309778942,-0.0081930587602151));
#25675=CARTESIAN_POINT('Ctrl Pts',(-2.12422647149672,59.0644081240037,-0.219475798871333));
#25676=CARTESIAN_POINT('Ctrl Pts',(-4.03709441305572,58.9597672746394,-1.0249483296966));
#25677=CARTESIAN_POINT('Ctrl Pts',(-4.90553716562939,58.9055357266085,-1.61159017972865));
#25678=CARTESIAN_POINT('Ctrl Pts',(-6.35728716070558,58.8001652751744,-3.07571052201888));
#25679=CARTESIAN_POINT('Ctrl Pts',(-6.93071050059505,58.7506869565062,-3.93533580739935));
#25680=CARTESIAN_POINT('Ctrl Pts',(-7.730857389611,58.643483347444,-5.8523875790016));
#25681=CARTESIAN_POINT('Ctrl Pts',(-7.93900584987437,58.5888280890297,-6.89564522768173));
#25682=CARTESIAN_POINT('Ctrl Pts',(-7.93601188136394,58.4862177532171,-8.97842987475304));
#25683=CARTESIAN_POINT('Ctrl Pts',(-7.73424899273246,58.432791164476,-9.99783257480142));
#25684=CARTESIAN_POINT('Ctrl Pts',(-6.95289199510558,58.3265026038045,-11.9024072243827));
#25685=CARTESIAN_POINT('Ctrl Pts',(-6.3807665232794,58.2767222658109,-12.7695853151988));
#25686=CARTESIAN_POINT('Ctrl Pts',(-4.9264068263455,58.1707986014925,-14.2482912875934));
#25687=CARTESIAN_POINT('Ctrl Pts',(-4.05382565662097,58.1162006356794,-14.8412769218402));
#25688=CARTESIAN_POINT('Ctrl Pts',(-2.14856615042794,58.0118723832767,-15.6469501937843));
#25689=CARTESIAN_POINT('Ctrl Pts',(-1.13736426870951,57.9613894163571,-15.859519147805));
#25690=CARTESIAN_POINT('Ctrl Pts',(-0.0757975649706369,57.9064245841019,
-15.8747286596535));
#25691=CARTESIAN_POINT('Ctrl Pts',(-0.0378925437277257,57.9044619724947,
-15.875));
#25692=CARTESIAN_POINT('Ctrl Pts',(-1.65020682103393E-14,57.9025000069372,
-15.875));
#25693=CARTESIAN_POINT('Ctrl Pts',(4.16333634234434E-14,57.585,-15.875));
#25694=CARTESIAN_POINT('Ctrl Pts',(-0.339782330037041,57.6025929394809,
-15.875));
#25695=CARTESIAN_POINT('Ctrl Pts',(-0.679929883044116,57.620204789143,-15.8531829030035));
#25696=CARTESIAN_POINT('Ctrl Pts',(-2.03597579501405,57.6904168971709,-15.677760512839));
#25697=CARTESIAN_POINT('Ctrl Pts',(-3.01846250588086,57.7398472625498,-15.3500371537862));
#25698=CARTESIAN_POINT('Ctrl Pts',(-4.81038415668122,57.8457912036368,-14.3352790937223));
#25699=CARTESIAN_POINT('Ctrl Pts',(-5.60146190223546,57.8996175171944,-13.6554687198988));
#25700=CARTESIAN_POINT('Ctrl Pts',(-6.88627321846298,58.003174129505,-12.0211764769394));
#25701=CARTESIAN_POINT('Ctrl Pts',(-7.36378911356066,58.0561003466381,-11.0794791319821));
#25702=CARTESIAN_POINT('Ctrl Pts',(-7.92025569096539,58.1631347809417,-9.08668634075335));
#25703=CARTESIAN_POINT('Ctrl Pts',(-8.00229948056471,58.2130736377048,-8.05710234326254));
#25704=CARTESIAN_POINT('Ctrl Pts',(-7.76885187234643,58.3178625581627,-6.00495505647574));
#25705=CARTESIAN_POINT('Ctrl Pts',(-7.44832322723047,58.3723383680281,-5.00283465188581));
#25706=CARTESIAN_POINT('Ctrl Pts',(-6.44323380849496,58.4777682604099,-3.18839246259855));
#25707=CARTESIAN_POINT('Ctrl Pts',(-5.7717540276406,58.5280100230615,-2.39168096627223));
#25708=CARTESIAN_POINT('Ctrl Pts',(-4.16543162801495,58.6345107045546,-1.10317396789013));
#25709=CARTESIAN_POINT('Ctrl Pts',(-3.24712380499084,58.6868733861705,-0.622126441379978));
#25710=CARTESIAN_POINT('Ctrl Pts',(-1.2552562525196,58.790006487002,-0.0297074686909277));
#25711=CARTESIAN_POINT('Ctrl Pts',(-0.198198163241447,58.8447378763312,
0.0668345080933514));
#25712=CARTESIAN_POINT('Ctrl Pts',(1.86583999797739,58.9516077610969,-0.15464714389086));
#25713=CARTESIAN_POINT('Ctrl Pts',(2.85402266121887,59.000990762468,-0.460286273074888));
#25714=CARTESIAN_POINT('Ctrl Pts',(4.66889230269638,59.1066891337393,-1.43539015288564));
#25715=CARTESIAN_POINT('Ctrl Pts',(5.47637777191838,59.1607166930885,-2.09922980586532));
#25716=CARTESIAN_POINT('Ctrl Pts',(6.79475781869968,59.264789534924,-3.70428102513771));
#25717=CARTESIAN_POINT('Ctrl Pts',(7.29106346199966,59.3168616505675,-4.63153621958218));
#25718=CARTESIAN_POINT('Ctrl Pts',(7.89194961574985,59.4237785969329,-6.60751033148493));
#25719=CARTESIAN_POINT('Ctrl Pts',(7.99752408848844,59.4741575859055,-7.63528348516183));
#25720=CARTESIAN_POINT('Ctrl Pts',(7.81065922498977,59.5785662358421,-9.69484408682032));
#25721=CARTESIAN_POINT('Ctrl Pts',(7.51192916122549,59.633146439635,-10.7061672575415));
#25722=CARTESIAN_POINT('Ctrl Pts',(6.54693177542636,59.7389904444348,-12.5420457180578));
#25723=CARTESIAN_POINT('Ctrl Pts',(5.89506370655858,59.7888356752205,-13.3515877405736));
#25724=CARTESIAN_POINT('Ctrl Pts',(4.31894432922972,59.8951692845151,-14.6761759419956));
#25725=CARTESIAN_POINT('Ctrl Pts',(3.4098803020298,59.9484463287595,-15.1787168423269));
#25726=CARTESIAN_POINT('Ctrl Pts',(1.64368893807556,60.0398945737998,-15.7467998769928));
#25727=CARTESIAN_POINT('Ctrl Pts',(0.823610448553,60.082355849624,-15.875));
#25728=CARTESIAN_POINT('Ctrl Pts',(1.0547118733939E-14,60.125,-15.875));
#25729=CARTESIAN_POINT('Origin',(0.,-18.001,-7.93750000000004));
#25730=CARTESIAN_POINT('',(-1.93598231170393E-14,62.9825000069372,-15.875));
#25731=CARTESIAN_POINT('',(2.011970106995E-15,62.665,-15.875));
#25732=CARTESIAN_POINT('',(-9.72063396823211E-16,-18.001,-15.875));
#25733=CARTESIAN_POINT('Ctrl Pts',(-3.15372727932584E-14,62.9825000069372,
-15.875));
#25734=CARTESIAN_POINT('Ctrl Pts',(0.202097295059188,62.9720359975791,-15.875));
#25735=CARTESIAN_POINT('Ctrl Pts',(0.404416516961662,62.9615604974959,-15.8672817297692));
#25736=CARTESIAN_POINT('Ctrl Pts',(1.63259922643455,62.8979687737096,-15.7731590536421));
#25737=CARTESIAN_POINT('Ctrl Pts',(2.63364172886998,62.8482064285161,-15.4957337446288));
#25738=CARTESIAN_POINT('Ctrl Pts',(4.48821271510264,62.7422597601501,-14.5671154837294));
#25739=CARTESIAN_POINT('Ctrl Pts',(5.32108159298415,62.6876568181105,-13.919307059151));
#25740=CARTESIAN_POINT('Ctrl Pts',(6.67410565714498,62.5833522595343,-12.3543254453134));
#25741=CARTESIAN_POINT('Ctrl Pts',(7.18756598284996,62.532837992169,-11.4575792833147));
#25742=CARTESIAN_POINT('Ctrl Pts',(7.85095345772089,62.4259538799676,-9.50257986084704));
#25743=CARTESIAN_POINT('Ctrl Pts',(7.98829852933518,62.3740857654634,-8.46088434379739));
#25744=CARTESIAN_POINT('Ctrl Pts',(7.85354132625254,62.2698825144621,-6.38856407192546));
#25745=CARTESIAN_POINT('Ctrl Pts',(7.5845388285196,62.2158063716604,-5.37781803848968));
#25746=CARTESIAN_POINT('Ctrl Pts',(6.67850515167161,62.1101775500444,-3.52715093599002));
#25747=CARTESIAN_POINT('Ctrl Pts',(6.05410047661468,62.0607874182207,-2.70285965881397));
#25748=CARTESIAN_POINT('Ctrl Pts',(4.50625049009188,61.9538361533165,-1.31906693082812));
#25749=CARTESIAN_POINT('Ctrl Pts',(3.59062340200669,61.8991019948323,-0.780853875088621));
#25750=CARTESIAN_POINT('Ctrl Pts',(1.62582918411219,61.7960985177442,-0.100652828940019));
#25751=CARTESIAN_POINT('Ctrl Pts',(0.59875659387989,61.7435018795739,0.0438133331380165));
#25752=CARTESIAN_POINT('Ctrl Pts',(-1.45730781215225,61.6370448526294,-0.0670459362428228));
#25753=CARTESIAN_POINT('Ctrl Pts',(-2.46661620655107,61.5869213186422,-0.322801609672158));
#25754=CARTESIAN_POINT('Ctrl Pts',(-4.34099082680039,61.4813776395764,-1.21092100594497));
#25755=CARTESIAN_POINT('Ctrl Pts',(-5.18610754905106,61.4268712647324,-1.83869869527229));
#25756=CARTESIAN_POINT('Ctrl Pts',(-6.57231654782088,61.322180938439,-3.37068079576465));
#25757=CARTESIAN_POINT('Ctrl Pts',(-7.10574521383588,61.2721368134212,-4.2551702600581));
#25758=CARTESIAN_POINT('Ctrl Pts',(-7.81464166704676,61.1651324282433,-6.19782536029372));
#25759=CARTESIAN_POINT('Ctrl Pts',(-7.97550281132237,61.1124453895675,-7.24019516760617));
#25760=CARTESIAN_POINT('Ctrl Pts',(-7.8848546839527,61.00874841751,-9.31656609692131));
#25761=CARTESIAN_POINT('Ctrl Pts',(-7.63840144165978,60.9548660605398,-10.3307035254926));
#25762=CARTESIAN_POINT('Ctrl Pts',(-6.77398691623051,60.8489844409294,-12.200027200501));
#25763=CARTESIAN_POINT('Ctrl Pts',(-6.16707844614086,60.7995781925467,-13.0387922031794));
#25764=CARTESIAN_POINT('Ctrl Pts',(-4.6504368530779,60.6929460987205,-14.4550522143311));
#25765=CARTESIAN_POINT('Ctrl Pts',(-3.7489923611215,60.6382321649877,-15.012121390154));
#25766=CARTESIAN_POINT('Ctrl Pts',(-1.87990224912114,60.5387968203394,-15.7068054476382));
#25767=CARTESIAN_POINT('Ctrl Pts',(-0.943373418127358,60.4913451350848,
-15.875));
#25768=CARTESIAN_POINT('Ctrl Pts',(-3.96904731303493E-14,60.4425000069372,
-15.875));
#25769=CARTESIAN_POINT('Ctrl Pts',(1.7277845820729E-14,60.125,-15.875));
#25770=CARTESIAN_POINT('Ctrl Pts',(-0.226288585779035,60.1367165639378,
-15.875));
#25771=CARTESIAN_POINT('Ctrl Pts',(-0.452843794342004,60.1484469328263,
-15.8653234055953));
#25772=CARTESIAN_POINT('Ctrl Pts',(-1.6992260327771,60.2129809752188,-15.7583040034926));
#25773=CARTESIAN_POINT('Ctrl Pts',(-2.6928575836504,60.2624313282865,-15.4741365811628));
#25774=CARTESIAN_POINT('Ctrl Pts',(-4.52949287564852,60.3678610680446,-14.5378172957273));
#25775=CARTESIAN_POINT('Ctrl Pts',(-5.35259392234133,60.4220600864358,-13.8898368067058));
#25776=CARTESIAN_POINT('Ctrl Pts',(-6.70314601741735,60.5266063575655,-12.3135105812172));
#25777=CARTESIAN_POINT('Ctrl Pts',(-7.21741767317199,60.5779632451856,-11.4002390114388));
#25778=CARTESIAN_POINT('Ctrl Pts',(-7.86089989495349,60.6847543784082,-9.44066014903061));
#25779=CARTESIAN_POINT('Ctrl Pts',(-7.98908164381013,60.735675385345,-8.41471175824484));
#25780=CARTESIAN_POINT('Ctrl Pts',(-7.84696393519802,60.8396891769703,-6.34863050227391));
#25781=CARTESIAN_POINT('Ctrl Pts',(-7.56932150876318,60.8943443121659,-5.32893387479916));
#25782=CARTESIAN_POINT('Ctrl Pts',(-6.64292842814975,61.0005570846869,-3.47302337167262));
#25783=CARTESIAN_POINT('Ctrl Pts',(-6.00974115202779,61.0501373773226,-2.65138266101345));
#25784=CARTESIAN_POINT('Ctrl Pts',(-4.46277146764076,61.15628161346,-1.29289580927297));
#25785=CARTESIAN_POINT('Ctrl Pts',(-3.56275523162316,61.2098978636032,-0.76992870869702));
#25786=CARTESIAN_POINT('Ctrl Pts',(-1.59559148720447,61.312946760467,-0.0914966241905969));
#25787=CARTESIAN_POINT('Ctrl Pts',(-0.545085500598828,61.3667770602637,
0.0505518195889912));
#25788=CARTESIAN_POINT('Ctrl Pts',(1.52401785543784,61.4739092060654,-0.0807414638915074));
#25789=CARTESIAN_POINT('Ctrl Pts',(2.52325426037719,61.5235497053457,-0.342468272518263));
#25790=CARTESIAN_POINT('Ctrl Pts',(4.38205626604549,61.6286677796305,-1.23803692927503));
#25791=CARTESIAN_POINT('Ctrl Pts',(5.22110593153846,61.6830204226522,-1.86911385571455));
#25792=CARTESIAN_POINT('Ctrl Pts',(6.60477821039722,61.7880316012073,-3.41513007765455));
#25793=CARTESIAN_POINT('Ctrl Pts',(7.13751660206741,61.838761541179,-4.31385899089811));
#25794=CARTESIAN_POINT('Ctrl Pts',(7.82490539208493,61.9454098588283,-6.25627151994931));
#25795=CARTESIAN_POINT('Ctrl Pts',(7.97643435265441,61.9970119853646,-7.28024705713402));
#25796=CARTESIAN_POINT('Ctrl Pts',(7.88049079223563,62.1005883383699,-9.35244792683858));
#25797=CARTESIAN_POINT('Ctrl Pts',(7.62474681542995,62.1552949485995,-10.3803051201895));
#25798=CARTESIAN_POINT('Ctrl Pts',(6.7382818869712,62.2618587950999,-12.256318494557));
#25799=CARTESIAN_POINT('Ctrl Pts',(6.12421616988546,62.3112826412378,-13.0902280433275));
#25800=CARTESIAN_POINT('Ctrl Pts',(4.60732456708991,62.4172119016502,-14.4830501085843));
#25801=CARTESIAN_POINT('Ctrl Pts',(3.7169602271815,62.4710517623904,-15.0266493449583));
#25802=CARTESIAN_POINT('Ctrl Pts',(1.86707321036374,62.569311797536,-15.7091456472123));
#25803=CARTESIAN_POINT('Ctrl Pts',(0.936777902232627,62.6164963684569,-15.875));
#25804=CARTESIAN_POINT('Ctrl Pts',(3.33066907387547E-15,62.665,-15.875));
#25805=CARTESIAN_POINT('Origin',(0.,-18.001,-7.93750000000004));
#25806=CARTESIAN_POINT('',(1.25243943714144E-14,65.5225000069373,-15.875));
#25807=CARTESIAN_POINT('',(1.66882607035807E-8,65.2049999982718,-15.875));
#25808=CARTESIAN_POINT('',(-9.72063396823211E-16,-18.001,-15.875));
#25809=CARTESIAN_POINT('Ctrl Pts',(1.33226762955019E-14,65.5225000069373,
-15.875));
#25810=CARTESIAN_POINT('Ctrl Pts',(0.31798534665268,65.5060356517754,-15.875));
#25811=CARTESIAN_POINT('Ctrl Pts',(0.636316449646511,65.4895533943575,-15.8558922241094));
#25812=CARTESIAN_POINT('Ctrl Pts',(1.97149062497534,65.4204219640669,-15.6943732610773));
#25813=CARTESIAN_POINT('Ctrl Pts',(2.95621850317269,65.3710202288267,-15.3750150925043));
#25814=CARTESIAN_POINT('Ctrl Pts',(4.77049532067681,65.2643670008657,-14.367720393661));
#25815=CARTESIAN_POINT('Ctrl Pts',(5.57801341588977,65.2096509963783,-13.6813045822467));
#25816=CARTESIAN_POINT('Ctrl Pts',(6.86449941164187,65.1061974727468,-12.0527046457698));
#25817=CARTESIAN_POINT('Ctrl Pts',(7.3383808086568,65.0543910989868,-11.1319720576279));
#25818=CARTESIAN_POINT('Ctrl Pts',(7.91170114059625,64.9477834231852,-9.15332177337935));
#25819=CARTESIAN_POINT('Ctrl Pts',(8.00264487832203,64.8972024958372,-8.1133662550448));
#25820=CARTESIAN_POINT('Ctrl Pts',(7.77989688373839,64.7920704222477,-6.05077387734165));
#25821=CARTESIAN_POINT('Ctrl Pts',(7.46585471838791,64.7376806043326,-5.0482921676172));
#25822=CARTESIAN_POINT('Ctrl Pts',(6.47715265519464,64.6326524598438,-3.23668389145497));
#25823=CARTESIAN_POINT('Ctrl Pts',(5.81779588770328,64.5829392756886,-2.44164728380225));
#25824=CARTESIAN_POINT('Ctrl Pts',(4.21402507587749,64.4758333815647,-1.12974213176186));
#25825=CARTESIAN_POINT('Ctrl Pts',(3.27881719531308,64.422267612215,-0.633215477804607));
#25826=CARTESIAN_POINT('Ctrl Pts',(1.28577089731952,64.3190734793731,-0.0371655150868924));
#25827=CARTESIAN_POINT('Ctrl Pts',(0.249068143622023,64.2653960300383,0.0628911822732485));
#25828=CARTESIAN_POINT('Ctrl Pts',(-1.79992259375097,64.1593052570558,-0.13882489303033));
#25829=CARTESIAN_POINT('Ctrl Pts',(-2.79296634004953,64.1097773484048,-0.436939094872029));
#25830=CARTESIAN_POINT('Ctrl Pts',(-4.62798300031585,64.0034697089433,-1.40433243496831));
#25831=CARTESIAN_POINT('Ctrl Pts',(-5.44861613942039,63.9487985565476,-2.07122317832839));
#25832=CARTESIAN_POINT('Ctrl Pts',(-6.769193390288,63.8448964529897,-3.66764005408777));
#25833=CARTESIAN_POINT('Ctrl Pts',(-7.26328380690333,63.7938089106022,-4.57617640678974));
#25834=CARTESIAN_POINT('Ctrl Pts',(-7.88256773057987,63.6870539327616,-6.54288354813264));
#25835=CARTESIAN_POINT('Ctrl Pts',(-7.99716772080512,63.6358723480358,-7.58379124967247));
#25836=CARTESIAN_POINT('Ctrl Pts',(-7.81943328777949,63.5312019187572,-9.65163458704426));
#25837=CARTESIAN_POINT('Ctrl Pts',(-7.52843743600606,63.4769603244062,-10.6585944507657));
#25838=CARTESIAN_POINT('Ctrl Pts',(-6.58196697346264,63.3716088285271,-12.490491058003));
#25839=CARTESIAN_POINT('Ctrl Pts',(-5.94050296954954,63.3221206920407,-13.3005597608152));
#25840=CARTESIAN_POINT('Ctrl Pts',(-4.36290956784409,63.2149223220041,-14.6515336183974));
#25841=CARTESIAN_POINT('Ctrl Pts',(-3.43460176955039,63.1603336837683,-15.1704922957151));
#25842=CARTESIAN_POINT('Ctrl Pts',(-1.64512523130868,63.0676798002179,-15.7465518933932));
#25843=CARTESIAN_POINT('Ctrl Pts',(-0.824409094713655,63.0251855088854,
-15.875));
#25844=CARTESIAN_POINT('Ctrl Pts',(-2.73392419813945E-14,62.9825000069372,
-15.875));
#25845=CARTESIAN_POINT('Ctrl Pts',(1.2490009027033E-15,62.665,-15.875));
#25846=CARTESIAN_POINT('Ctrl Pts',(-0.10678118416443,62.6705288187308,-15.875));
#25847=CARTESIAN_POINT('Ctrl Pts',(-0.213647259459413,62.6760620328766,
-15.872845270232));
#25848=CARTESIAN_POINT('Ctrl Pts',(-1.34302158695393,62.7345377464097,-15.8272013626226));
#25849=CARTESIAN_POINT('Ctrl Pts',(-2.34792454259774,62.7845009481365,-15.5885368982462));
#25850=CARTESIAN_POINT('Ctrl Pts',(-4.22888299835772,62.8892664994659,-14.7350472466522));
#25851=CARTESIAN_POINT('Ctrl Pts',(-5.08391034054569,62.943749794255,-14.1216687243596));
#25852=CARTESIAN_POINT('Ctrl Pts',(-6.50106978542234,63.0492070983699,-12.6070847518793));
#25853=CARTESIAN_POINT('Ctrl Pts',(-7.05246541554818,63.0994197763401,-11.7232139155279));
#25854=CARTESIAN_POINT('Ctrl Pts',(-7.7843363065139,63.2059100881859,-9.79846319705741));
#25855=CARTESIAN_POINT('Ctrl Pts',(-7.95956486650432,63.2583279998295,-8.77658404257087));
#25856=CARTESIAN_POINT('Ctrl Pts',(-7.91042328869039,63.3614302547978,-6.69880402378148));
#25857=CARTESIAN_POINT('Ctrl Pts',(-7.67700460042873,63.4161624749171,-5.66317283210756));
#25858=CARTESIAN_POINT('Ctrl Pts',(-6.83110447614055,63.523052036865,-3.7673646936249));
#25859=CARTESIAN_POINT('Ctrl Pts',(-6.23626917479286,63.5724360057793,-2.9212286952175));
#25860=CARTESIAN_POINT('Ctrl Pts',(-4.75000240174356,63.6781179028192,-1.49438308178774));
#25861=CARTESIAN_POINT('Ctrl Pts',(-3.86977713807099,63.7321572644408,-0.93027336542813));
#25862=CARTESIAN_POINT('Ctrl Pts',(-1.93699135180268,63.8362615476154,-0.169845992183665));
#25863=CARTESIAN_POINT('Ctrl Pts',(-0.902252022585847,63.8882840179527,
0.0170235810373091));
#25864=CARTESIAN_POINT('Ctrl Pts',(1.16254452587274,63.995193169801,-0.0191477078170207));
#25865=CARTESIAN_POINT('Ctrl Pts',(2.17298276010862,64.0456038399461,-0.234906896833842));
#25866=CARTESIAN_POINT('Ctrl Pts',(4.07531544991997,64.1499877049775,-1.04643591649846));
#25867=CARTESIAN_POINT('Ctrl Pts',(4.94578121005329,64.2045735311781,-1.6419342765105));
#25868=CARTESIAN_POINT('Ctrl Pts',(6.3956331167362,64.3104423616632,-3.1250429491433));
#25869=CARTESIAN_POINT('Ctrl Pts',(6.96524562977749,64.3602669442802,-3.99425454748881));
#25870=CARTESIAN_POINT('Ctrl Pts',(7.74066191783563,64.4665897807739,-5.90145550622931));
#25871=CARTESIAN_POINT('Ctrl Pts',(7.93913616305028,64.5199274320883,-6.92118389939431));
#25872=CARTESIAN_POINT('Ctrl Pts',(7.93580414760589,64.6225360324781,-9.00382346629569));
#25873=CARTESIAN_POINT('Ctrl Pts',(7.72434917474791,64.6772676622739,-10.0465791137209));
#25874=CARTESIAN_POINT('Ctrl Pts',(6.91824317872534,64.7844469600654,-11.9612009534146));
#25875=CARTESIAN_POINT('Ctrl Pts',(6.342091661726,64.8339051380756,-12.8191145522525));
#25876=CARTESIAN_POINT('Ctrl Pts',(4.88592030297376,64.9393173518797,-14.2785216455929));
#25877=CARTESIAN_POINT('Ctrl Pts',(4.01594808771533,64.9935261647386,-14.8623113341349));
#25878=CARTESIAN_POINT('Ctrl Pts',(2.10051462720201,65.0981007259448,-15.6620746218592));
#25879=CARTESIAN_POINT('Ctrl Pts',(1.07350198982203,65.1494171933907,-15.8702705442612));
#25880=CARTESIAN_POINT('Ctrl Pts',(0.0237043088711802,65.2037726599216,
-15.8749734566493));
#25881=CARTESIAN_POINT('Ctrl Pts',(0.0118515279162405,65.2043863624004,
-15.8749999999751));
#25882=CARTESIAN_POINT('Ctrl Pts',(1.67328657821244E-8,65.2049999991336,
-15.875));
#25883=CARTESIAN_POINT('Origin',(0.,-18.001,-7.93750000000004));
#25884=CARTESIAN_POINT('',(-9.12495460877611E-15,68.0625000069372,-15.875));
#25885=CARTESIAN_POINT('',(-1.87381047919305E-15,67.745,-15.875));
#25886=CARTESIAN_POINT('',(-9.72063396823211E-16,-18.001,-15.875));
#25887=CARTESIAN_POINT('Ctrl Pts',(-1.80411241501588E-14,68.0625000069372,
-15.875));
#25888=CARTESIAN_POINT('Ctrl Pts',(0.433688074095033,68.0400449015164,-15.875));
#25889=CARTESIAN_POINT('Ctrl Pts',(0.867646658930349,68.0175757898376,-15.8394569362102));
#25890=CARTESIAN_POINT('Ctrl Pts',(2.30744279971092,67.9430273388727,-15.6008963918652));
#25891=CARTESIAN_POINT('Ctrl Pts',(3.27552241898614,67.8935284260736,-15.2397501722207));
#25892=CARTESIAN_POINT('Ctrl Pts',(5.04600416610042,67.7863355943929,-14.1544463263054));
#25893=CARTESIAN_POINT('Ctrl Pts',(5.82518660607671,67.7318161969776,-13.4310630253555));
#25894=CARTESIAN_POINT('Ctrl Pts',(7.04237597061802,67.6291349825518,-11.7413550114365));
#25895=CARTESIAN_POINT('Ctrl Pts',(7.47592761909007,67.5756772732154,-10.7966330639291));
#25896=CARTESIAN_POINT('Ctrl Pts',(7.95782719209122,67.4694103717858,-8.79519864354836));
#25897=CARTESIAN_POINT('Ctrl Pts',(8.00189302295181,67.4196664096423,-7.75749681019158));
#25898=CARTESIAN_POINT('Ctrl Pts',(7.68906167925432,67.3136957724166,-5.70714517179668));
#25899=CARTESIAN_POINT('Ctrl Pts',(7.32892036503718,67.2590877202392,-4.71521019537982));
#25900=CARTESIAN_POINT('Ctrl Pts',(6.25607408933573,67.1548080819376,-2.94614230636956));
#25901=CARTESIAN_POINT('Ctrl Pts',(5.56078284775951,67.1042605791076,-2.18164713990146));
#25902=CARTESIAN_POINT('Ctrl Pts',(3.9048740859986,66.9973843651778,-0.949050596015295));
#25903=CARTESIAN_POINT('Ctrl Pts',(2.95619879843677,66.9455633712056,-0.497926058022581));
#25904=CARTESIAN_POINT('Ctrl Pts',(0.943071919052903,66.8413295243412,0.0116014630028445));
#25905=CARTESIAN_POINT('Ctrl Pts',(-0.101548405123127,66.7872421262658,
0.0666974313818716));
#25906=CARTESIAN_POINT('Ctrl Pts',(-2.14129294923519,66.6816300942421,-0.225927537827141));
#25907=CARTESIAN_POINT('Ctrl Pts',(-3.11766848499563,66.6322370806252,-0.566366463438777));
#25908=CARTESIAN_POINT('Ctrl Pts',(-4.91070117103948,66.5252668143996,-1.61331850571048));
#25909=CARTESIAN_POINT('Ctrl Pts',(-5.70465454808869,66.4705322689865,-2.31901377130391));
#25910=CARTESIAN_POINT('Ctrl Pts',(-6.95653847210559,66.3675598567049,-3.97943092341129));
#25911=CARTESIAN_POINT('Ctrl Pts',(-7.41003568161736,66.314906435902,-4.91235547833897));
#25912=CARTESIAN_POINT('Ctrl Pts',(-7.93705275327936,66.2084599009704,-6.90277823869244));
#25913=CARTESIAN_POINT('Ctrl Pts',(-8.00421592914212,66.1583631665413,-7.94164872216537));
#25914=CARTESIAN_POINT('Ctrl Pts',(-7.73591046461968,66.0527927576801,-9.99834006578266));
#25915=CARTESIAN_POINT('Ctrl Pts',(-7.39854633601598,65.9982793995688,-10.9957528004814));
#25916=CARTESIAN_POINT('Ctrl Pts',(-6.36722845879569,65.8936128524359,-12.7861712278592));
#25917=CARTESIAN_POINT('Ctrl Pts',(-5.68972391939372,65.8435423580799,-13.5658425210553));
#25918=CARTESIAN_POINT('Ctrl Pts',(-4.05955075944524,65.7365452666697,-14.8378328977529));
#25919=CARTESIAN_POINT('Ctrl Pts',(-3.11747828465378,65.683913953298,-15.3114860958317));
#25920=CARTESIAN_POINT('Ctrl Pts',(-1.4218679409655,65.5961201879295,-15.7792475927008));
#25921=CARTESIAN_POINT('Ctrl Pts',(-0.711800218347542,65.5593549492248,
-15.875));
#25922=CARTESIAN_POINT('Ctrl Pts',(1.20736753927986E-14,65.5225000069373,
-15.875));
#25923=CARTESIAN_POINT('Ctrl Pts',(1.67328666200728E-8,65.2049999991336,
-15.875));
#25924=CARTESIAN_POINT('Ctrl Pts',(-1.01235319717274,65.2574167002126,-15.8750000021342));
#25925=CARTESIAN_POINT('Ctrl Pts',(-2.01552439406243,65.3077533698532,-15.6813225282047));
#25926=CARTESIAN_POINT('Ctrl Pts',(-3.92677583366418,65.4111468805206,-14.9146103708258));
#25927=CARTESIAN_POINT('Ctrl Pts',(-4.81164344365151,65.4658058045133,-14.3365325951033));
#25928=CARTESIAN_POINT('Ctrl Pts',(-6.29233096466331,65.572040262209,-12.8838516545358));
#25929=CARTESIAN_POINT('Ctrl Pts',(-6.87914313474992,65.6216079664635,-12.0286110836041));
#25930=CARTESIAN_POINT('Ctrl Pts',(-7.69561202403318,65.727740263692,-10.1386182960918));
#25931=CARTESIAN_POINT('Ctrl Pts',(-7.91621294150844,65.7813705506426,-9.12119984513197));
#25932=CARTESIAN_POINT('Ctrl Pts',(-7.95620178249735,65.8844525831829,-7.04085658844557));
#25933=CARTESIAN_POINT('Ctrl Pts',(-7.76810461068915,65.9382221328197,-5.9978958009839));
#25934=CARTESIAN_POINT('Ctrl Pts',(-7.00660948082297,66.0453484056575,-4.06985581544896));
#25935=CARTESIAN_POINT('Ctrl Pts',(-6.45012112291448,66.0950046272612,-3.19965036604002));
#25936=CARTESIAN_POINT('Ctrl Pts',(-5.02596225176608,66.2001024717331,-1.7065114721996));
#25937=CARTESIAN_POINT('Ctrl Pts',(-4.16719289431384,66.2544637285815,-1.10229333846056));
#25938=CARTESIAN_POINT('Ctrl Pts',(-2.27042579493747,66.3595025670694,-0.261582695513758));
#25939=CARTESIAN_POINT('Ctrl Pts',(-1.25155999052137,66.4101978686835,-0.0312918302746155));
#25940=CARTESIAN_POINT('Ctrl Pts',(0.80802194173164,66.5168370228915,0.0250971154595979));
#25941=CARTESIAN_POINT('Ctrl Pts',(1.8290296902527,66.568484833832,-0.145818051007626));
#25942=CARTESIAN_POINT('Ctrl Pts',(3.77137211901572,66.6720334348404,-0.874833121602433));
#25943=CARTESIAN_POINT('Ctrl Pts',(4.67076854080747,66.7267423476151,-1.43455624455437));
#25944=CARTESIAN_POINT('Ctrl Pts',(6.18293899381204,66.8333267158754,-2.85540207612083));
#25945=CARTESIAN_POINT('Ctrl Pts',(6.78734513232732,66.8827447931084,-3.69622717082995));
#25946=CARTESIAN_POINT('Ctrl Pts',(7.64579728348592,66.9886599454099,-5.568169103159));
#25947=CARTESIAN_POINT('Ctrl Pts',(7.88902800709171,67.0425126204529,-6.58275082634948));
#25948=CARTESIAN_POINT('Ctrl Pts',(7.97336727667615,67.1461349622059,-8.65965607432826));
#25949=CARTESIAN_POINT('Ctrl Pts',(7.80912783457669,67.1989485584348,-9.70211051669221));
#25950=CARTESIAN_POINT('Ctrl Pts',(7.09370088741321,67.305969091227,-11.6429716481885));
#25951=CARTESIAN_POINT('Ctrl Pts',(6.5574081612622,67.3559559570471,-12.5256946078923));
#25952=CARTESIAN_POINT('Ctrl Pts',(5.16646318780928,67.4606991356996,-14.052894831553));
#25953=CARTESIAN_POINT('Ctrl Pts',(4.31962152002127,67.5151894545751,-14.6777707668926));
#25954=CARTESIAN_POINT('Ctrl Pts',(2.44243730461787,67.6206727411499,-15.5600386989748));
#25955=CARTESIAN_POINT('Ctrl Pts',(1.43194224651504,67.6708582008068,-15.8126574641793));
#25956=CARTESIAN_POINT('Ctrl Pts',(0.267589531288932,67.7311449933869,-15.8716202456688));
#25957=CARTESIAN_POINT('Ctrl Pts',(0.133733921363328,67.7380756470332,-15.875));
#25958=CARTESIAN_POINT('Ctrl Pts',(-1.58900670399476E-14,67.745,-15.875));
#25959=CARTESIAN_POINT('Origin',(0.,-18.001,-7.93750000000004));
#25960=CARTESIAN_POINT('',(-3.57703071997799E-14,70.6025000069373,-15.875));
#25961=CARTESIAN_POINT('',(-3.747311833248E-15,70.2850000000001,-15.875));
#25962=CARTESIAN_POINT('',(-9.72063396823211E-16,-18.001,-15.875));
#25963=CARTESIAN_POINT('Ctrl Pts',(-7.34134975033385E-14,70.6025000069373,
-15.875));
#25964=CARTESIAN_POINT('Ctrl Pts',(0.55468147166431,70.5737802157667,-15.875));
#25965=CARTESIAN_POINT('Ctrl Pts',(1.10917310827725,70.5450702537025,-15.8168567412127));
#25966=CARTESIAN_POINT('Ctrl Pts',(2.65519167658246,70.4650219147983,-15.4874140063886));
#25967=CARTESIAN_POINT('Ctrl Pts',(3.60546903429097,70.414923428072,-15.0825560851003));
#25968=CARTESIAN_POINT('Ctrl Pts',(5.31698959833044,70.3079339887368,-13.922782238041));
#25969=CARTESIAN_POINT('Ctrl Pts',(6.05728423695684,70.2553602068774,-13.1722964105403));
#25970=CARTESIAN_POINT('Ctrl Pts',(7.19946640267268,70.1515957220018,-11.4362185862728));
#25971=CARTESIAN_POINT('Ctrl Pts',(7.59355757884135,70.0976867479508,-10.4695111044688));
#25972=CARTESIAN_POINT('Ctrl Pts',(7.98719067824395,69.9918362508845,-8.44785329199879));
#25973=CARTESIAN_POINT('Ctrl Pts',(7.98625615382667,69.9424387179082,-7.41272651414423));
#25974=CARTESIAN_POINT('Ctrl Pts',(7.5859664650825,69.8357635883035,-5.37648534904374));
#25975=CARTESIAN_POINT('Ctrl Pts',(7.18118656516031,69.7810455393853,-4.3968205716101));
#25976=CARTESIAN_POINT('Ctrl Pts',(6.02712129486966,69.6776229024158,-2.67154587193301));
#25977=CARTESIAN_POINT('Ctrl Pts',(5.29670537170189,69.6257643506818,-1.93736593228556));
#25978=CARTESIAN_POINT('Ctrl Pts',(3.59037049556738,69.5191669285006,-0.783335574039568));
#25979=CARTESIAN_POINT('Ctrl Pts',(2.62899582321277,69.4686217540813,-0.376995500569623));
#25980=CARTESIAN_POINT('Ctrl Pts',(0.597945629743748,69.3634598902127,0.0455639264374251));
#25981=CARTESIAN_POINT('Ctrl Pts',(-0.452688703198433,69.3090611042784,
0.0551154855814628));
#25982=CARTESIAN_POINT('Ctrl Pts',(-2.4807164905748,69.204055731795,-0.328479105333356));
#25983=CARTESIAN_POINT('Ctrl Pts',(-3.44000422234571,69.1543230279237,-0.711332810312225));
#25984=CARTESIAN_POINT('Ctrl Pts',(-5.18134004871023,69.0472238382526,-1.83367566723749));
#25985=CARTESIAN_POINT('Ctrl Pts',(-5.94127210539138,68.9937228453009,-2.57057409498428));
#25986=CARTESIAN_POINT('Ctrl Pts',(-7.12155151995333,68.8904927597585,-4.28342106841755));
#25987=CARTESIAN_POINT('Ctrl Pts',(-7.53576398510425,68.836800292985,-5.23919402969178));
#25988=CARTESIAN_POINT('Ctrl Pts',(-7.97417133547815,68.7307232145494,-7.25090510299311));
#25989=CARTESIAN_POINT('Ctrl Pts',(-7.99602537296488,68.6812071389458,-8.28738315381936));
#25990=CARTESIAN_POINT('Ctrl Pts',(-7.64013578098366,68.5748760894848,-10.3310633838858));
#25991=CARTESIAN_POINT('Ctrl Pts',(-7.25799660543989,68.520201211879,-11.3172078780045));
#25992=CARTESIAN_POINT('Ctrl Pts',(-6.14510573557978,68.4163273726159,-13.0650237333758));
#25993=CARTESIAN_POINT('Ctrl Pts',(-5.43255623533737,68.365196845588,-13.8146819879853));
#25994=CARTESIAN_POINT('Ctrl Pts',(-3.75180666418746,68.2584510528248,-15.0088026868805));
#25995=CARTESIAN_POINT('Ctrl Pts',(-2.79683739267014,68.2073121017327,-15.4379700976919));
#25996=CARTESIAN_POINT('Ctrl Pts',(-1.1992115311013,68.1245916874823,-15.8069975347168));
#25997=CARTESIAN_POINT('Ctrl Pts',(-0.599864530783218,68.0935592453197,
-15.875));
#25998=CARTESIAN_POINT('Ctrl Pts',(-1.92901250528621E-14,68.0625000069372,
-15.875));
#25999=CARTESIAN_POINT('Ctrl Pts',(-2.05391259555654E-14,67.745,-15.875));
#26000=CARTESIAN_POINT('Ctrl Pts',(-0.891384039551465,67.7911532695368,
-15.875));
#26001=CARTESIAN_POINT('Ctrl Pts',(-1.7773915122855,67.8364542179145,-15.7248304672442));
#26002=CARTESIAN_POINT('Ctrl Pts',(-3.61297397000325,67.9328823135545,-15.0828398530554));
#26003=CARTESIAN_POINT('Ctrl Pts',(-4.52663207304087,67.9876152259936,-14.5419576646853));
#26004=CARTESIAN_POINT('Ctrl Pts',(-6.07012261666185,68.0945233969593,-13.1535806673219));
#26005=CARTESIAN_POINT('Ctrl Pts',(-6.69207962534341,68.1439087193146,-12.3272575904096));
#26006=CARTESIAN_POINT('Ctrl Pts',(-7.59229918481167,68.2495748379419,-10.4739439583062));
#26007=CARTESIAN_POINT('Ctrl Pts',(-7.85814601219587,68.3036253291705,-9.46269350425099));
#26008=CARTESIAN_POINT('Ctrl Pts',(-7.98673368238065,68.4077593993229,-7.38977351839877));
#26009=CARTESIAN_POINT('Ctrl Pts',(-7.84611012968646,68.459735104669,-6.34797524464098));
#26010=CARTESIAN_POINT('Ctrl Pts',(-7.17637265411212,68.5666368012141,-4.39468196874761));
#26011=CARTESIAN_POINT('Ctrl Pts',(-6.6601250121187,68.6170780294673,-3.49964044689932));
#26012=CARTESIAN_POINT('Ctrl Pts',(-5.30245198461667,68.7214382324708,-1.93922920673743));
#26013=CARTESIAN_POINT('Ctrl Pts',(-4.46785065444924,68.7760293035196,-1.2941953574911));
#26014=CARTESIAN_POINT('Ctrl Pts',(-2.61049320716362,68.8819216103495,-0.371198553129155));
#26015=CARTESIAN_POINT('Ctrl Pts',(-1.60829789989605,68.9317270186858,-0.0967770647009433));
#26016=CARTESIAN_POINT('Ctrl Pts',(0.444976416468158,69.0380395829131,0.0540955344220655));
#26017=CARTESIAN_POINT('Ctrl Pts',(1.47642819725269,69.091435194494,-0.0709120054369154));
#26018=CARTESIAN_POINT('Ctrl Pts',(3.45719629546723,69.1940137749849,-0.715165556475455));
#26019=CARTESIAN_POINT('Ctrl Pts',(4.3843592522318,69.2487445829194,-1.23739075811436));
#26020=CARTESIAN_POINT('Ctrl Pts',(5.95793719659881,69.3559400751924,-2.59379686046367));
#26021=CARTESIAN_POINT('Ctrl Pts',(6.59681536733345,69.4054060723789,-3.40602830215141));
#26022=CARTESIAN_POINT('Ctrl Pts',(7.53716663208879,69.5108015548906,-5.24080641497974));
#26023=CARTESIAN_POINT('Ctrl Pts',(7.82482937244818,69.56501957705,-6.24837058041258));
#26024=CARTESIAN_POINT('Ctrl Pts',(7.99605244940215,69.6696208830364,-8.31692586567543));
#26025=CARTESIAN_POINT('Ctrl Pts',(7.87801665925337,69.7208993945324,-9.35796079940542));
#26026=CARTESIAN_POINT('Ctrl Pts',(7.25206501843802,69.8276746720165,-11.3229137027457));
#26027=CARTESIAN_POINT('Ctrl Pts',(6.75504492769195,69.8786681783344,-12.2296730844804));
#26028=CARTESIAN_POINT('Ctrl Pts',(5.42954504333603,69.9826329032435,-13.821372161045));
#26029=CARTESIAN_POINT('Ctrl Pts',(4.60703967623432,70.0372953340462,-14.4853994278399));
#26030=CARTESIAN_POINT('Ctrl Pts',(2.76904453052918,70.1435502549678,-15.4469609983921));
#26031=CARTESIAN_POINT('Ctrl Pts',(1.77479255518857,70.1931064103273,-15.7419667278455));
#26032=CARTESIAN_POINT('Ctrl Pts',(0.501572705197605,70.2590300260852,-15.8631284936286));
#26033=CARTESIAN_POINT('Ctrl Pts',(0.250642322080538,70.2720224705234,-15.875));
#26034=CARTESIAN_POINT('Ctrl Pts',(-5.20417042793042E-15,70.2850000000001,
-15.875));
#26035=CARTESIAN_POINT('Origin',(0.,-18.001,-7.93750000000004));
#26036=CARTESIAN_POINT('',(-9.72063396823211E-16,73.0000000000001,-15.875));
#26037=CARTESIAN_POINT('',(1.12292432555688E-15,72.825,-15.875));
#26038=CARTESIAN_POINT('',(-9.72063396823211E-16,-18.001,-15.875));
#26039=CARTESIAN_POINT('',(2.74837297199504,73.,-15.3839993290006));
#26040=CARTESIAN_POINT('Origin',(0.,73.,-7.93749999999999));
#26041=CARTESIAN_POINT('Ctrl Pts',(2.74837297199475,73.0000000000001,-15.3839993290008));
#26042=CARTESIAN_POINT('Ctrl Pts',(3.59437464131025,72.9550594340577,-15.0717548743275));
#26043=CARTESIAN_POINT('Ctrl Pts',(4.38096265156832,72.9082896699512,-14.6176303844275));
#26044=CARTESIAN_POINT('Ctrl Pts',(5.76270270874511,72.815450657477,-13.4689100881607));
#26045=CARTESIAN_POINT('Ctrl Pts',(6.34930118539488,72.7715825043545,-12.7843132261676));
#26046=CARTESIAN_POINT('Ctrl Pts',(7.3429699107917,72.6739979374842,-11.1254790275496));
#26047=CARTESIAN_POINT('Ctrl Pts',(7.69663294708784,72.6197352866454,-10.1384533621628));
#26048=CARTESIAN_POINT('Ctrl Pts',(8.00161174031953,72.5144245725012,-8.09895165090422));
#26049=CARTESIAN_POINT('Ctrl Pts',(7.95572988529432,72.4649139308815,-7.06676082021326));
#26050=CARTESIAN_POINT('Ctrl Pts',(7.46768900153107,72.357726908696,-5.04863649787649));
#26051=CARTESIAN_POINT('Ctrl Pts',(7.01922926841232,72.3032788768853,-4.08499423286156));
#26052=CARTESIAN_POINT('Ctrl Pts',(5.78611525301393,72.200560231844,-2.4070808512331));
#26053=CARTESIAN_POINT('Ctrl Pts',(5.02049908302566,72.1470861581906,-1.70379959241594));
#26054=CARTESIAN_POINT('Ctrl Pts',(3.26437485118427,72.0408309468112,-0.629542832290954));
#26055=CARTESIAN_POINT('Ctrl Pts',(2.29069621884348,71.9911055858172,-0.268398105084747));
#26056=CARTESIAN_POINT('Ctrl Pts',(0.243547344159033,71.8851101791205,0.064821270957295));
#26057=CARTESIAN_POINT('Ctrl Pts',(-0.81122908592498,71.8304969274595,0.0273254603393398));
#26058=CARTESIAN_POINT('Ctrl Pts',(-2.82473809981346,71.7262432947834,-0.449305473372096));
#26059=CARTESIAN_POINT('Ctrl Pts',(-3.76609380580235,71.6756607697004,-0.875717113837374));
#26060=CARTESIAN_POINT('Ctrl Pts',(-5.44815635567005,71.5687928129177,-2.0720447416791));
#26061=CARTESIAN_POINT('Ctrl Pts',(-6.16910522104993,71.5170203032762,-2.83573318331477));
#26062=CARTESIAN_POINT('Ctrl Pts',(-7.27331242840743,71.4127547779465,-4.59432468902859));
#26063=CARTESIAN_POINT('Ctrl Pts',(-7.64719722588607,71.3586557850724,-5.571456424903));
#26064=CARTESIAN_POINT('Ctrl Pts',(-7.99631495195053,71.2530613299722,-7.60237859159013));
#26065=CARTESIAN_POINT('Ctrl Pts',(-7.97278718391001,71.203664836868,-8.63607257488857));
#26066=CARTESIAN_POINT('Ctrl Pts',(-7.52827571758297,71.0966749348865,-10.6643374475176));
#26067=CARTESIAN_POINT('Ctrl Pts',(-7.10100257500505,71.041940096802,-11.6370346730576));
#26068=CARTESIAN_POINT('Ctrl Pts',(-5.90604744264877,70.9390001163971,-13.3392219121527));
#26069=CARTESIAN_POINT('Ctrl Pts',(-5.15775556231888,70.8862871268732,-14.0577905255233));
#26070=CARTESIAN_POINT('Ctrl Pts',(-3.42595037494629,70.7798515578262,-15.1714458061015));
#26071=CARTESIAN_POINT('Ctrl Pts',(-2.45827221640794,70.7297821829296,-15.554851267113));
#26072=CARTESIAN_POINT('Ctrl Pts',(-0.966818965162028,70.6525590772289,
-15.8308526453184));
#26073=CARTESIAN_POINT('Ctrl Pts',(-0.483337411686185,70.6275258104618,
-15.875));
#26074=CARTESIAN_POINT('Ctrl Pts',(-7.39686090156511E-14,70.6025000069373,
-15.875));
#26075=CARTESIAN_POINT('Ctrl Pts',(-5.13478148889135E-15,70.2850000000001,
-15.875));
#26076=CARTESIAN_POINT('Ctrl Pts',(-0.777177421330428,70.3252399834562,
-15.875));
#26077=CARTESIAN_POINT('Ctrl Pts',(-1.55158524899007,70.365336565418,-15.7608488491832));
#26078=CARTESIAN_POINT('Ctrl Pts',(-3.30231265475548,70.4559841317402,-15.2312860424146));
#26079=CARTESIAN_POINT('Ctrl Pts',(-4.23649762123155,70.5096965065944,-14.7313986180527));
#26080=CARTESIAN_POINT('Ctrl Pts',(-5.83636493185836,70.6168171685367,-13.4136355136902));
#26081=CARTESIAN_POINT('Ctrl Pts',(-6.49304723000878,70.6664887070802,-12.6163446127004));
#26082=CARTESIAN_POINT('Ctrl Pts',(-7.47544971294546,70.7715672857524,-10.8016652876116));
#26083=CARTESIAN_POINT('Ctrl Pts',(-7.78604964647708,70.8259366083522,-9.79848133719328));
#26084=CARTESIAN_POINT('Ctrl Pts',(-8.00207469181669,70.9310015342891,-7.73506814054177));
#26085=CARTESIAN_POINT('Ctrl Pts',(-7.90760817690709,70.9816644604433,-6.69496258235393));
#26086=CARTESIAN_POINT('Ctrl Pts',(-7.32743704232001,71.0882948993028,-4.71807599845438));
#26087=CARTESIAN_POINT('Ctrl Pts',(-6.8505419701571,71.1399863614486,-3.79915534071941));
#26088=CARTESIAN_POINT('Ctrl Pts',(-5.55895784608872,71.2435085992257,-2.1753145531283));
#26089=CARTESIAN_POINT('Ctrl Pts',(-4.74946229624585,71.2982196009796,-1.49178485530757));
#26090=CARTESIAN_POINT('Ctrl Pts',(-2.93207164078339,71.4048232854104,-0.490403897681004));
#26091=CARTESIAN_POINT('Ctrl Pts',(-1.94610588454118,71.4542363050593,-0.174191892264601));
#26092=CARTESIAN_POINT('Ctrl Pts',(0.0992332456347186,71.5601380084559,
0.0663966627234519));
#26093=CARTESIAN_POINT('Ctrl Pts',(1.13955264224962,71.614002717028,-0.0145088029096499));
#26094=CARTESIAN_POINT('Ctrl Pts',(3.14145196896345,71.7176552339138,-0.573609583815303));
#26095=CARTESIAN_POINT('Ctrl Pts',(4.08252146116871,71.7704174893548,-1.05063963155032));
#26096=CARTESIAN_POINT('Ctrl Pts',(5.70881450440919,71.8774315400999,-2.32852778385979));
#26097=CARTESIAN_POINT('Ctrl Pts',(6.38364567440301,71.9274412025371,-3.11047008078335));
#26098=CARTESIAN_POINT('Ctrl Pts',(7.40870062480463,72.0321631297841,-4.90404808705329));
#26099=CARTESIAN_POINT('Ctrl Pts',(7.74263369637828,72.0866599944385,-5.90224069919674));
#26100=CARTESIAN_POINT('Ctrl Pts',(8.00423542243036,72.1921677292453,-7.95983746731116));
#26101=CARTESIAN_POINT('Ctrl Pts',(7.93358266755552,72.242327892559,-8.99887486620816));
#26102=CARTESIAN_POINT('Ctrl Pts',(7.39976478850669,72.3487988845475,-10.9875845715094));
#26103=CARTESIAN_POINT('Ctrl Pts',(6.9432719145105,72.4013202714971,-11.9187244089226));
#26104=CARTESIAN_POINT('Ctrl Pts',(5.68629056082371,72.5043651493195,-13.5745066378289));
#26105=CARTESIAN_POINT('Ctrl Pts',(4.89032358003968,72.5590986277707,-14.2773953572043));
#26106=CARTESIAN_POINT('Ctrl Pts',(3.09414933749014,72.6660242711992,-15.3185571933526));
#26107=CARTESIAN_POINT('Ctrl Pts',(2.11654896885027,72.7154112585455,-15.65591967121));
#26108=CARTESIAN_POINT('Ctrl Pts',(0.736312332434618,72.786875891833,-15.8493886519877));
#26109=CARTESIAN_POINT('Ctrl Pts',(0.368139781712966,72.8059387942585,-15.875));
#26110=CARTESIAN_POINT('Ctrl Pts',(-6.24500451351651E-16,72.825,-15.875));
#26111=CARTESIAN_POINT('Origin',(0.,0.,-3.));
#26112=CARTESIAN_POINT('',(7.42417289639114,16.3976113139839,-3.));
#26113=CARTESIAN_POINT('',(-7.42417289639223,16.3976113139834,-3.));
#26114=CARTESIAN_POINT('Origin',(0.,0.,-3.));
#26115=CARTESIAN_POINT('',(6.18681074697836,13.6646760949931,0.));
#26116=CARTESIAN_POINT('Origin',(6.18681074698069,13.6646760949919,-2.99999999999878));
#26117=CARTESIAN_POINT('',(-6.18681074697897,13.6646760949927,0.));
#26118=CARTESIAN_POINT('Origin',(0.,0.,0.));
#26119=CARTESIAN_POINT('Origin',(-6.18681074697897,13.6646760949927,-3.));
#26120=CARTESIAN_POINT('Origin',(0.,1.11022302462516E-13,-12.875));
#26121=CARTESIAN_POINT('',(6.18681074697913,13.6646760949928,-15.875));
#26122=CARTESIAN_POINT('',(-6.18681074697824,13.6646760949932,-15.875));
#26123=CARTESIAN_POINT('Origin',(0.,1.11022302462516E-13,-15.875));
#26124=CARTESIAN_POINT('',(7.42417289637494,16.3976113139913,-12.8749999999944));
#26125=CARTESIAN_POINT('Origin',(6.18681074697913,13.6646760949928,-12.875));
#26126=CARTESIAN_POINT('',(-7.42417289638977,16.3976113139846,-12.875));
#26127=CARTESIAN_POINT('Origin',(0.,1.11022302462516E-13,-12.875));
#26128=CARTESIAN_POINT('Origin',(-6.18681074697824,13.6646760949932,-12.875));
#26129=CARTESIAN_POINT('Origin',(0.,1.11022302462516E-13,-15.875));
#26130=CARTESIAN_POINT('',(-9.,1.09920120343283E-13,-15.875));
#26131=CARTESIAN_POINT('Origin',(0.,1.11022302462516E-13,-15.875));
#26132=CARTESIAN_POINT('',(-9.,1.09920120343283E-13,0.));
#26133=CARTESIAN_POINT('',(-9.,1.09920120343283E-13,-15.875));
#26134=CARTESIAN_POINT('Origin',(0.,0.,0.));
#26135=CARTESIAN_POINT('Origin',(0.,1.11022302462516E-13,-15.875));
#26136=CARTESIAN_POINT('Ctrl Pts',(7.42417484634227,16.3976156207155,-12.87499999998));
#26137=CARTESIAN_POINT('Ctrl Pts',(7.49425297313204,16.3658856681913,-12.751333844329));
#26138=CARTESIAN_POINT('Ctrl Pts',(7.56155134995267,16.3348713727113,-12.6261535808136));
#26139=CARTESIAN_POINT('Ctrl Pts',(7.62612254669854,16.3046697269754,-12.4994671770732));
#26140=CARTESIAN_POINT('Ctrl Pts',(7.75422681491928,16.2447519939762,-12.2481311346493));
#26141=CARTESIAN_POINT('Ctrl Pts',(7.8715970357136,16.1880292793325,-11.9908686844778));
#26142=CARTESIAN_POINT('Ctrl Pts',(7.97820798185054,16.1353117293752,-11.7274704800121));
#26143=CARTESIAN_POINT('Ctrl Pts',(8.01721016407619,16.1160257220333,-11.6311097859114));
#26144=CARTESIAN_POINT('Ctrl Pts',(8.05478002264463,16.0972716532196,-11.533899256748));
#26145=CARTESIAN_POINT('Ctrl Pts',(8.09090985732795,16.0790913201412,-11.4358370389061));
#26146=CARTESIAN_POINT('Ctrl Pts',(8.16205634437451,16.0432908011739,-11.2427339601735));
#26147=CARTESIAN_POINT('Ctrl Pts',(8.22753637682579,16.0097534434489,-11.0461762836229));
#26148=CARTESIAN_POINT('Ctrl Pts',(8.28688853410253,15.9789727293006,-10.8478320212478));
#26149=CARTESIAN_POINT('Ctrl Pts',(8.32131121783912,15.9611207280098,-10.7327975873204));
#26150=CARTESIAN_POINT('Ctrl Pts',(8.35367325807109,15.9441955973044,-10.6171617077227));
#26151=CARTESIAN_POINT('Ctrl Pts',(8.38388984996585,15.928290085497,-10.5012445343995));
#26152=CARTESIAN_POINT('Ctrl Pts',(8.40113973300348,15.9192100337397,-10.4350703712496));
#26153=CARTESIAN_POINT('Ctrl Pts',(8.41770873842301,15.9104526090396,-10.3687432766716));
#26154=CARTESIAN_POINT('Ctrl Pts',(8.43357670502026,15.9020371015176,-10.3023247062374));
#26155=CARTESIAN_POINT('Ctrl Pts',(8.48142109323413,15.8766630369558,-10.102062382203));
#26156=CARTESIAN_POINT('Ctrl Pts',(8.523181690265,15.8542538078078,-9.90026706475298));
#26157=CARTESIAN_POINT('Ctrl Pts',(8.55878117848867,15.8350118244306,-9.69708852759311));
#26158=CARTESIAN_POINT('Ctrl Pts',(8.58582632375289,15.8203935739563,-9.54273257119468));
#26159=CARTESIAN_POINT('Ctrl Pts',(8.60931643956188,15.807602915796,-9.38757857490814));
#26160=CARTESIAN_POINT('Ctrl Pts',(8.62923459807846,15.7967193688509,-9.23169795700352));
#26161=CARTESIAN_POINT('Ctrl Pts',(8.63350792596552,15.794384365611,-9.19825465495383));
#26162=CARTESIAN_POINT('Ctrl Pts',(8.63761733451759,15.7921368728815,-9.16477496999481));
#26163=CARTESIAN_POINT('Ctrl Pts',(8.64156280552917,15.7899775895407,-9.13125885731573));
#26164=CARTESIAN_POINT('Ctrl Pts',(8.66292988244127,15.7782837833811,-8.94974913254405));
#26165=CARTESIAN_POINT('Ctrl Pts',(8.67947376513277,15.76917652596,-8.7671681095378));
#26166=CARTESIAN_POINT('Ctrl Pts',(8.69110604433138,15.762762383104,-8.58349117024342));
#26167=CARTESIAN_POINT('Ctrl Pts',(8.69218421804267,15.7621678684702,-8.56646650603642));
#26168=CARTESIAN_POINT('Ctrl Pts',(8.69322014673618,15.7615965171088,-8.54943307927023));
#26169=CARTESIAN_POINT('Ctrl Pts',(8.69421378566647,15.7610483994286,-8.53239054158288));
#26170=CARTESIAN_POINT('Ctrl Pts',(8.70328572291703,15.7560440773868,-8.37679193551244));
#26171=CARTESIAN_POINT('Ctrl Pts',(8.70880616372846,15.7529912511763,-8.2201332575878));
#26172=CARTESIAN_POINT('Ctrl Pts',(8.7107488498173,15.7519163037688,-8.06401072201215));
#26173=CARTESIAN_POINT('Ctrl Pts',(8.71131293962653,15.7516041756893,-8.01867806028393));
#26174=CARTESIAN_POINT('Ctrl Pts',(8.7115750876793,15.75145896852,-7.97339056290001));
#26175=CARTESIAN_POINT('Ctrl Pts',(8.71153392734093,15.7514817282356,-7.92818743022105));
#26176=CARTESIAN_POINT('Ctrl Pts',(8.71153351011403,15.7514819589423,-7.92772922304078));
#26177=CARTESIAN_POINT('Ctrl Pts',(8.71153306168016,15.7514822069308,-7.92727102504393));
#26178=CARTESIAN_POINT('Ctrl Pts',(8.71153258203798,15.7514824722023,-7.92681283627777));
#26179=CARTESIAN_POINT('Ctrl Pts',(8.71107948717309,15.7517330613572,-7.49398398029794));
#26180=CARTESIAN_POINT('Ctrl Pts',(8.68356072203589,15.7672456706329,-7.06559071877813));
#26181=CARTESIAN_POINT('Ctrl Pts',(8.62923684404765,15.7968989356927,-6.6415377335116));
#26182=CARTESIAN_POINT('Ctrl Pts',(8.58285778982776,15.8222154344209,-6.27950215865738));
#26183=CARTESIAN_POINT('Ctrl Pts',(8.51694114102254,15.8578381576886,-5.92062950477275));
#26184=CARTESIAN_POINT('Ctrl Pts',(8.43166005791346,15.903053441183,-5.56483757189164));
#26185=CARTESIAN_POINT('Ctrl Pts',(8.41576539569238,15.9114806519099,-5.49852518011659));
#26186=CARTESIAN_POINT('Ctrl Pts',(8.39916523028649,15.920251577545,-5.43228961453733));
#26187=CARTESIAN_POINT('Ctrl Pts',(8.38188287493475,15.9293455250075,-5.36619796746088));
#26188=CARTESIAN_POINT('Ctrl Pts',(8.33068896116534,15.9562836797177,-5.17042082872912));
#26189=CARTESIAN_POINT('Ctrl Pts',(8.27345820241746,15.9860834909743,-4.97580581749668));
#26190=CARTESIAN_POINT('Ctrl Pts',(8.21073783355088,16.0182329075637,-4.7840118256463));
#26191=CARTESIAN_POINT('Ctrl Pts',(8.17202073055818,16.0380786497962,-4.66561794706999));
#26192=CARTESIAN_POINT('Ctrl Pts',(8.13121144680357,16.0588197898457,-4.54829977429853));
#26193=CARTESIAN_POINT('Ctrl Pts',(8.08843644345115,16.0803356899397,-4.43245745460993));
#26194=CARTESIAN_POINT('Ctrl Pts',(8.05247016426092,16.0984267900955,-4.33505437137372));
#26195=CARTESIAN_POINT('Ctrl Pts',(8.01507184801902,16.1170887814765,-4.23846402227408));
#26196=CARTESIAN_POINT('Ctrl Pts',(7.97623595783032,16.1362866611022,-4.14266100529827));
#26197=CARTESIAN_POINT('Ctrl Pts',(7.86998595823516,16.1888095900877,-3.88055627522936));
#26198=CARTESIAN_POINT('Ctrl Pts',(7.75305710254994,16.2453053838483,-3.62448042379799));
#26199=CARTESIAN_POINT('Ctrl Pts',(7.62546188869204,16.3049787177716,-3.3742362248388));
#26200=CARTESIAN_POINT('Ctrl Pts',(7.561098085643,16.3350801815788,-3.2480036817129));
#26201=CARTESIAN_POINT('Ctrl Pts',(7.4940202195112,16.3659910561043,-3.12325541650477));
#26202=CARTESIAN_POINT('Ctrl Pts',(7.42417484827014,16.3976156249738,-3.00000000002115));
#26203=CARTESIAN_POINT('Ctrl Pts',(-7.42417484634355,16.3976156207149,-3.00000000002217));
#26204=CARTESIAN_POINT('Ctrl Pts',(-7.49425297313284,16.3658856681909,-3.12366615567247));
#26205=CARTESIAN_POINT('Ctrl Pts',(-7.56155134995302,16.3348713727112,-3.24884641918707));
#26206=CARTESIAN_POINT('Ctrl Pts',(-7.6261225466986,16.3046697269754,-3.37553282292674));
#26207=CARTESIAN_POINT('Ctrl Pts',(-7.75422681491959,16.2447519939761,-3.62686886535078));
#26208=CARTESIAN_POINT('Ctrl Pts',(-7.87159703571355,16.1880292793326,-3.88413131552216));
#26209=CARTESIAN_POINT('Ctrl Pts',(-7.97820798185047,16.1353117293752,-4.14752951998797));
#26210=CARTESIAN_POINT('Ctrl Pts',(-8.01721016407612,16.1160257220333,-4.24389021408868));
#26211=CARTESIAN_POINT('Ctrl Pts',(-8.05478002264456,16.0972716532196,-4.34110074325211));
#26212=CARTESIAN_POINT('Ctrl Pts',(-8.09090985732791,16.0790913201412,-4.43916296109398));
#26213=CARTESIAN_POINT('Ctrl Pts',(-8.1620563443761,16.0432908011731,-4.63226603983073));
#26214=CARTESIAN_POINT('Ctrl Pts',(-8.22753637682865,16.0097534434475,-4.82882371638596));
#26215=CARTESIAN_POINT('Ctrl Pts',(-8.28688853410642,15.9789727292985,-5.0271679787657));
#26216=CARTESIAN_POINT('Ctrl Pts',(-8.32131121784147,15.9611207280085,-5.14220241268877));
#26217=CARTESIAN_POINT('Ctrl Pts',(-8.35367325807209,15.9441955973039,-5.25783829228192));
#26218=CARTESIAN_POINT('Ctrl Pts',(-8.3838898499657,15.928290085497,-5.37375546560053));
#26219=CARTESIAN_POINT('Ctrl Pts',(-8.40113973300336,15.9192100337397,-5.43992962875046));
#26220=CARTESIAN_POINT('Ctrl Pts',(-8.41770873842293,15.9104526090397,-5.50625672332849));
#26221=CARTESIAN_POINT('Ctrl Pts',(-8.43357670502022,15.9020371015176,-5.57267529376267));
#26222=CARTESIAN_POINT('Ctrl Pts',(-8.48142109322884,15.8766630369586,-5.77293761777444));
#26223=CARTESIAN_POINT('Ctrl Pts',(-8.52318169025573,15.8542538078128,-5.97473293520173));
#26224=CARTESIAN_POINT('Ctrl Pts',(-8.55878117847675,15.835011824437,-6.17791147233861));
#26225=CARTESIAN_POINT('Ctrl Pts',(-8.58582632374597,15.8203935739601,-6.33226742875959));
#26226=CARTESIAN_POINT('Ctrl Pts',(-8.60931643955891,15.8076029157976,-6.48742142506895));
#26227=CARTESIAN_POINT('Ctrl Pts',(-8.62923459807841,15.796719368851,-6.64330204299652));
#26228=CARTESIAN_POINT('Ctrl Pts',(-8.63350792596547,15.794384365611,-6.67674534504622));
#26229=CARTESIAN_POINT('Ctrl Pts',(-8.63761733451752,15.7921368728815,-6.71022503000525));
#26230=CARTESIAN_POINT('Ctrl Pts',(-8.6415628055291,15.7899775895407,-6.74374114268435));
#26231=CARTESIAN_POINT('Ctrl Pts',(-8.66292988244114,15.7782837833812,-6.92525086745615));
#26232=CARTESIAN_POINT('Ctrl Pts',(-8.67947376513277,15.76917652596,-7.10783189046224));
#26233=CARTESIAN_POINT('Ctrl Pts',(-8.69110604433138,15.762762383104,-7.29150882975662));
#26234=CARTESIAN_POINT('Ctrl Pts',(-8.69218421804268,15.7621678684702,-7.30853349396362));
#26235=CARTESIAN_POINT('Ctrl Pts',(-8.69322014673619,15.7615965171088,-7.32556692072984));
#26236=CARTESIAN_POINT('Ctrl Pts',(-8.69421378566647,15.7610483994286,-7.3426094584172));
#26237=CARTESIAN_POINT('Ctrl Pts',(-8.70328572291651,15.7560440773871,-7.49820806447887));
#26238=CARTESIAN_POINT('Ctrl Pts',(-8.70880616372783,15.7529912511766,-7.65486674239446));
#26239=CARTESIAN_POINT('Ctrl Pts',(-8.71074884981696,15.751916303769,-7.81098927796124));
#26240=CARTESIAN_POINT('Ctrl Pts',(-8.71131293962642,15.7516041756893,-7.85632193969836));
#26241=CARTESIAN_POINT('Ctrl Pts',(-8.71157508767931,15.75145896852,-7.90160943709117));
#26242=CARTESIAN_POINT('Ctrl Pts',(-8.71153392734093,15.7514817282356,-7.94681256977899));
#26243=CARTESIAN_POINT('Ctrl Pts',(-8.71153351011403,15.7514819589423,-7.94727077695927));
#26244=CARTESIAN_POINT('Ctrl Pts',(-8.71153306168016,15.7514822069308,-7.94772897495614));
#26245=CARTESIAN_POINT('Ctrl Pts',(-8.71153258203797,15.7514824722023,-7.94818716372231));
#26246=CARTESIAN_POINT('Ctrl Pts',(-8.71107948717285,15.7517330613573,-8.38101601992454));
#26247=CARTESIAN_POINT('Ctrl Pts',(-8.68356072200785,15.7672456706487,-8.80940928166221));
#26248=CARTESIAN_POINT('Ctrl Pts',(-8.62923684396425,15.7968989357382,-9.23346226714217));
#26249=CARTESIAN_POINT('Ctrl Pts',(-8.58285778974884,15.8222154344636,-9.5954978417747));
#26250=CARTESIAN_POINT('Ctrl Pts',(-8.5169411409716,15.8578381577156,-9.95437049544148));
#26251=CARTESIAN_POINT('Ctrl Pts',(-8.43166005791337,15.9030534411831,-10.3101624281084));
#26252=CARTESIAN_POINT('Ctrl Pts',(-8.41576539569222,15.91148065191,-10.3764748198834));
#26253=CARTESIAN_POINT('Ctrl Pts',(-8.39916523028629,15.9202515775451,-10.4427103854627));
#26254=CARTESIAN_POINT('Ctrl Pts',(-8.38188287493453,15.9293455250077,-10.5088020325391));
#26255=CARTESIAN_POINT('Ctrl Pts',(-8.330688961164,15.9562836797184,-10.7045791712749));
#26256=CARTESIAN_POINT('Ctrl Pts',(-8.27345820241499,15.9860834909756,-10.8991941825113));
#26257=CARTESIAN_POINT('Ctrl Pts',(-8.21073783354696,16.0182329075658,-11.0909881743656));
#26258=CARTESIAN_POINT('Ctrl Pts',(-8.17202073055547,16.0380786497975,-11.2093820529379));
#26259=CARTESIAN_POINT('Ctrl Pts',(-8.13121144680218,16.0588197898464,-11.3267002257054));
#26260=CARTESIAN_POINT('Ctrl Pts',(-8.08843644345111,16.0803356899398,-11.4425425453902));
#26261=CARTESIAN_POINT('Ctrl Pts',(-8.05247016426082,16.0984267900955,-11.5399456286264));
#26262=CARTESIAN_POINT('Ctrl Pts',(-8.01507184801894,16.1170887814765,-11.636535977726));
#26263=CARTESIAN_POINT('Ctrl Pts',(-7.97623595783027,16.1362866611023,-11.7323389947018));
#26264=CARTESIAN_POINT('Ctrl Pts',(-7.86998595823514,16.1888095900877,-11.9944437247707));
#26265=CARTESIAN_POINT('Ctrl Pts',(-7.75305710255021,16.2453053838482,-12.2505195762024));
#26266=CARTESIAN_POINT('Ctrl Pts',(-7.62546188869214,16.3049787177716,-12.5007637751614));
#26267=CARTESIAN_POINT('Ctrl Pts',(-7.56109808564288,16.3350801815789,-12.6269963182875));
#26268=CARTESIAN_POINT('Ctrl Pts',(-7.49402021951091,16.3659910561045,-12.7517445834959));
#26269=CARTESIAN_POINT('Ctrl Pts',(-7.42417484826972,16.397615624974,-12.8749999999798));
#26270=CARTESIAN_POINT('Origin',(0.,76.,-7.93749999999999));
#26271=CARTESIAN_POINT('Ctrl Pts',(-5.80913668152293,74.3748153225003,-10.9908197002073));
#26272=CARTESIAN_POINT('Ctrl Pts',(-5.67334876482947,74.3157933474344,-11.3760244264246));
#26273=CARTESIAN_POINT('Ctrl Pts',(-5.48207182842344,74.2522007025348,-11.7998901094902));
#26274=CARTESIAN_POINT('Ctrl Pts',(-4.95384740584261,74.1135707631099,-12.653829766117));
#26275=CARTESIAN_POINT('Ctrl Pts',(-4.66538309328688,74.0478644569286,-13.0286302410656));
#26276=CARTESIAN_POINT('Ctrl Pts',(-3.74940791549978,73.8635536093087,-13.9963130606203));
#26277=CARTESIAN_POINT('Ctrl Pts',(-3.04622404223991,73.7476300383179,-14.5060716837974));
#26278=CARTESIAN_POINT('Ctrl Pts',(-1.74204887561165,73.5661588961296,-15.1231710302632));
#26279=CARTESIAN_POINT('Ctrl Pts',(-0.926330645356949,73.4550883535588,
-15.4378592293412));
#26280=CARTESIAN_POINT('Ctrl Pts',(0.562811661989643,73.2654430613796,-15.6006444679771));
#26281=CARTESIAN_POINT('Ctrl Pts',(0.991359300347177,73.2120251146354,-15.6108736298658));
#26282=CARTESIAN_POINT('Ctrl Pts',(1.86955409604265,73.1046785119871,-15.5571416466731));
#26283=CARTESIAN_POINT('Ctrl Pts',(2.31069667091151,73.0527156300785,-15.4893464683708));
#26284=CARTESIAN_POINT('Ctrl Pts',(2.74837297199499,73.0000000000003,-15.3839993290003));
#26285=CARTESIAN_POINT('',(-3.34416379521191,73.0000000000002,-15.1361439529118));
#26286=CARTESIAN_POINT('Origin',(0.,73.,-7.93749999999999));
#26287=CARTESIAN_POINT('',(-1.41388501872634E-15,73.694202182856,-0.694202182856027));
#26288=CARTESIAN_POINT('Ctrl Pts',(-3.34416379521187,73.,-15.1361439529117));
#26289=CARTESIAN_POINT('Ctrl Pts',(-4.22508208124688,73.0317651468065,-14.6918837683));
#26290=CARTESIAN_POINT('Ctrl Pts',(-5.01478929567479,73.0646106900317,-14.0862063128347));
#26291=CARTESIAN_POINT('Ctrl Pts',(-6.36082539665937,73.1306089592706,-12.580136728871));
#26292=CARTESIAN_POINT('Ctrl Pts',(-6.89299777093761,73.1630625007004,-11.6798119029563));
#26293=CARTESIAN_POINT('Ctrl Pts',(-7.59352950420832,73.2354722402261,-9.64199315526779));
#26294=CARTESIAN_POINT('Ctrl Pts',(-7.67550414883065,73.2681752177959,-8.65873837058869));
#26295=CARTESIAN_POINT('Ctrl Pts',(-7.60286970509253,73.3261655212376,-6.87515120113955));
#26296=CARTESIAN_POINT('Ctrl Pts',(-7.36420970282702,73.3605784477511,-5.89355743635864));
#26297=CARTESIAN_POINT('Ctrl Pts',(-6.56006614657876,73.4260174028793,-4.16903668548547));
#26298=CARTESIAN_POINT('Ctrl Pts',(-5.99694992288785,73.4580449578172,-3.34369296659196));
#26299=CARTESIAN_POINT('Ctrl Pts',(-4.85823706235724,73.5114865221786,-2.30042237137467));
#26300=CARTESIAN_POINT('Ctrl Pts',(-4.47064145492997,73.5284750019196,-2.0095633605085));
#26301=CARTESIAN_POINT('Ctrl Pts',(-3.24491645562334,73.5789367752769,-1.26504415519658));
#26302=CARTESIAN_POINT('Ctrl Pts',(-2.33864132871221,73.6108820263253,-0.928923923375816));
#26303=CARTESIAN_POINT('Ctrl Pts',(-0.933384219456304,73.6607444411162,
-0.70569357476857));
#26304=CARTESIAN_POINT('Ctrl Pts',(-0.465894690246344,73.6774433167434,
-0.677443316743452));
#26305=CARTESIAN_POINT('Ctrl Pts',(-1.38777878078145E-16,73.694202182856,
-0.694202182856026));
#26306=CARTESIAN_POINT('',(-6.04669357079005E-16,76.,-2.99999999999999));
#26307=CARTESIAN_POINT('',(-6.04669357079005E-16,76.,-2.99999999999999));
#26308=CARTESIAN_POINT('Origin',(0.,76.,-7.93749999999999));
#26309=CARTESIAN_POINT('Ctrl Pts',(2.77555756156289E-16,73.694202182856,
-0.694202182856026));
#26310=CARTESIAN_POINT('Ctrl Pts',(0.454376060453808,73.7105467081775,-0.710546708177571));
#26311=CARTESIAN_POINT('Ctrl Pts',(0.907235171861323,73.726948314343,-0.769702150673434));
#26312=CARTESIAN_POINT('Ctrl Pts',(2.26893059456179,73.7766019097737,-1.08089595715675));
#26313=CARTESIAN_POINT('Ctrl Pts',(3.13748436394977,73.8088335460852,-1.46722967249179));
#26314=CARTESIAN_POINT('Ctrl Pts',(4.7286962188268,73.8805074247047,-2.60266444957381));
#26315=CARTESIAN_POINT('Ctrl Pts',(5.35369283675739,73.9143938763295,-3.31453476733563));
#26316=CARTESIAN_POINT('Ctrl Pts',(6.25899628022628,73.975690028823,-4.7679037847388));
#26317=CARTESIAN_POINT('Ctrl Pts',(6.57538939670816,74.0084067304685,-5.58569923670778));
#26318=CARTESIAN_POINT('Ctrl Pts',(6.88151449957619,74.0722484654855,-7.25660344054492));
#26319=CARTESIAN_POINT('Ctrl Pts',(6.89995184173098,74.1046959288186,-8.18342538444765));
#26320=CARTESIAN_POINT('Ctrl Pts',(6.49722993178434,74.1755027990535,-10.0042182724129));
#26321=CARTESIAN_POINT('Ctrl Pts',(6.14535741819483,74.2094533637712,-10.8118598844939));
#26322=CARTESIAN_POINT('Ctrl Pts',(5.31863856072002,74.264263195562,-12.0097425581265));
#26323=CARTESIAN_POINT('Ctrl Pts',(4.9281190222573,74.2858035323405,-12.4428896711152));
#26324=CARTESIAN_POINT('Ctrl Pts',(4.05499771184754,74.3304865900484,-13.1839033554255));
#26325=CARTESIAN_POINT('Ctrl Pts',(3.58197878378907,74.3527482881805,-13.4911923382182));
#26326=CARTESIAN_POINT('Ctrl Pts',(3.07575458898223,74.3748153225001,-13.734789356643));
#26327=CARTESIAN_POINT('Origin',(0.,-18.001,-7.93750000000004));
#26328=CARTESIAN_POINT('Ctrl Pts',(-8.32667268468867E-16,72.825,-15.875));
#26329=CARTESIAN_POINT('Ctrl Pts',(-0.395827506290079,72.8454947954835,
-15.875));
#26330=CARTESIAN_POINT('Ctrl Pts',(-0.791617129110936,72.8659876294712,
-15.8453912454244));
#26331=CARTESIAN_POINT('Ctrl Pts',(-1.93136566829669,72.9250004894723,-15.6734516698727));
#26332=CARTESIAN_POINT('Ctrl Pts',(-2.65872844411335,72.9615973108245,-15.4545661585517));
#26333=CARTESIAN_POINT('Ctrl Pts',(-3.34416379521214,73.0000000000001,-15.1361439529117));
#26334=CARTESIAN_POINT('Origin',(0.,1.11022302462516E-13,-15.875));
#26335=CARTESIAN_POINT('',(-2.57755123502973,16.6150404676652,-15.875));
#26336=CARTESIAN_POINT('Ctrl Pts',(-6.18681074697824,13.6646760949932,-15.875));
#26337=CARTESIAN_POINT('Ctrl Pts',(-6.04942753338936,13.7268776392074,-15.875));
#26338=CARTESIAN_POINT('Ctrl Pts',(-5.91423497782962,13.7936520594916,-15.875));
#26339=CARTESIAN_POINT('Ctrl Pts',(-5.78131071258862,13.8644897336605,-15.875));
#26340=CARTESIAN_POINT('Ctrl Pts',(-5.64040818509895,13.9395791638243,-15.875));
#26341=CARTESIAN_POINT('Ctrl Pts',(-5.50205371352212,14.019234808701,-15.875));
#26342=CARTESIAN_POINT('Ctrl Pts',(-5.36636167242817,14.1029047612554,-15.875));
#26343=CARTESIAN_POINT('Ctrl Pts',(-5.29440248962166,14.1472759812823,-15.875));
#26344=CARTESIAN_POINT('Ctrl Pts',(-5.22319249151731,14.1927770029562,-15.875));
#26345=CARTESIAN_POINT('Ctrl Pts',(-5.15275208328258,14.2393303034111,-15.875));
#26346=CARTESIAN_POINT('Ctrl Pts',(-4.82417650905228,14.4564823303883,-15.875));
#26347=CARTESIAN_POINT('Ctrl Pts',(-4.51455185467379,14.6945381516704,-15.875));
#26348=CARTESIAN_POINT('Ctrl Pts',(-4.21891718821225,14.9480256152924,-15.875));
#26349=CARTESIAN_POINT('Ctrl Pts',(-3.62764785528917,15.4550005425365,-15.875));
#26350=CARTESIAN_POINT('Ctrl Pts',(-3.09286826794447,16.0242864292497,-15.875));
#26351=CARTESIAN_POINT('Ctrl Pts',(-2.57755123502973,16.6150404676652,-15.875));
#26352=CARTESIAN_POINT('Ctrl Pts',(-2.57755123503017,16.6150404676659,-15.875));
#26353=CARTESIAN_POINT('Ctrl Pts',(-2.53648329737381,16.6621203203971,-15.875));
#26354=CARTESIAN_POINT('Ctrl Pts',(-2.49248343900961,16.7057360650919,-15.875));
#26355=CARTESIAN_POINT('Ctrl Pts',(-2.44700266076792,16.7475590170876,-15.875));
#26356=CARTESIAN_POINT('Ctrl Pts',(-2.4020906969716,16.788858901973,-15.875));
#26357=CARTESIAN_POINT('Ctrl Pts',(-2.35562102859357,16.8282993969611,-15.875));
#26358=CARTESIAN_POINT('Ctrl Pts',(-2.3080370454668,16.8664261008931,-15.8749999999998));
#26359=CARTESIAN_POINT('Ctrl Pts',(-2.30742826936455,16.8669138832241,-15.8749999999998));
#26360=CARTESIAN_POINT('Ctrl Pts',(-2.30681931537933,16.8674014466309,-15.8749999999998));
#26361=CARTESIAN_POINT('Ctrl Pts',(-2.30621018438793,16.8678887923135,-15.8749999999998));
#26362=CARTESIAN_POINT('Ctrl Pts',(-2.23061417258728,16.9283706763259,-15.8749999999995));
#26363=CARTESIAN_POINT('Ctrl Pts',(-2.15212082757854,16.9856522751252,-15.875));
#26364=CARTESIAN_POINT('Ctrl Pts',(-2.0718228292108,17.0403639484817,-15.8749999999997));
#26365=CARTESIAN_POINT('Ctrl Pts',(-2.05098109666076,17.054564627037,-15.8749999999996));
#26366=CARTESIAN_POINT('Ctrl Pts',(-2.03001761816751,17.0685919387124,-15.8749999999995));
#26367=CARTESIAN_POINT('Ctrl Pts',(-2.00895126657008,17.0824564612662,-15.8749999999992));
#26368=CARTESIAN_POINT('Ctrl Pts',(-2.00765800896842,17.0833076005394,-15.8749999999992));
#26369=CARTESIAN_POINT('Ctrl Pts',(-2.00636435367826,17.0841581316114,-15.8749999999992));
#26370=CARTESIAN_POINT('Ctrl Pts',(-2.00507030581251,17.0850080563855,-15.8749999999992));
#26371=CARTESIAN_POINT('Ctrl Pts',(-1.90188935724152,17.1527768358274,-15.8749999999978));
#26372=CARTESIAN_POINT('Ctrl Pts',(-1.796434748319,17.2164714546352,-15.8749999999985));
#26373=CARTESIAN_POINT('Ctrl Pts',(-1.68924216461426,17.2770977324932,-15.8749999999992));
#26374=CARTESIAN_POINT('Ctrl Pts',(-1.58388083753985,17.3366882831633,-15.8749999999998));
#26375=CARTESIAN_POINT('Ctrl Pts',(-1.47682790841131,17.3932876269073,-15.8749999999999));
#26376=CARTESIAN_POINT('Ctrl Pts',(-1.36838950083533,17.4474158111803,-15.8749999999999));
#26377=CARTESIAN_POINT('Ctrl Pts',(-1.36701527573572,17.4481017702523,-15.8749999999999));
#26378=CARTESIAN_POINT('Ctrl Pts',(-1.36564083943549,17.4487873299025,-15.8749999999999));
#26379=CARTESIAN_POINT('Ctrl Pts',(-1.36426619268609,17.4494724911175,-15.8749999999999));
#26380=CARTESIAN_POINT('Ctrl Pts',(-1.24440837618391,17.5092128769371,-15.8749999999996));
#26381=CARTESIAN_POINT('Ctrl Pts',(-1.12295905583498,17.5659434337456,-15.8749999999586));
#26382=CARTESIAN_POINT('Ctrl Pts',(-1.00026331620377,17.6199805908429,-15.8749999998258));
#26383=CARTESIAN_POINT('Ctrl Pts',(-0.898709167959604,17.6647066545109,
-15.874999999716));
#26384=CARTESIAN_POINT('Ctrl Pts',(-0.796301966219198,17.7075888044325,
-15.874999999598));
#26385=CARTESIAN_POINT('Ctrl Pts',(-0.693249644331463,17.7488301778621,
-15.8749999996073));
#26386=CARTESIAN_POINT('Ctrl Pts',(-0.550308584896857,17.8060349598853,
-15.8749999996201));
#26387=CARTESIAN_POINT('Ctrl Pts',(-0.406059151969994,17.8600031401019,
-15.8749999998645));
#26388=CARTESIAN_POINT('Ctrl Pts',(-0.261072807205695,17.911130219345,-15.8749999999505));
#26389=CARTESIAN_POINT('Ctrl Pts',(-0.174270671136077,17.9417395825683,
-15.8750000000021));
#26390=CARTESIAN_POINT('Ctrl Pts',(-0.0872048169539691,17.9713317586215,
-15.875));
#26391=CARTESIAN_POINT('Ctrl Pts',(5.82643290799559E-14,18.0000000000001,
-15.875));
#26392=CARTESIAN_POINT('',(2.57755123502973,16.6150404676651,-15.875));
#26393=CARTESIAN_POINT('Ctrl Pts',(6.56141807553468E-14,18.0000000000001,
-15.875));
#26394=CARTESIAN_POINT('Ctrl Pts',(0.163234899420945,17.9463369294279,-15.875));
#26395=CARTESIAN_POINT('Ctrl Pts',(0.325479452729011,17.8896359397147,-15.8749999997925));
#26396=CARTESIAN_POINT('Ctrl Pts',(0.486261202262205,17.829207831248,-15.8749999978486));
#26397=CARTESIAN_POINT('Ctrl Pts',(0.556197005496128,17.8029232043187,-15.8749999970031));
#26398=CARTESIAN_POINT('Ctrl Pts',(0.625856192700561,17.7759340687492,-15.8749999959428));
#26399=CARTESIAN_POINT('Ctrl Pts',(0.695200618726449,17.7481866429567,-15.8749999948273));
#26400=CARTESIAN_POINT('Ctrl Pts',(0.695202869078957,17.7481857425023,-15.8749999948272));
#26401=CARTESIAN_POINT('Ctrl Pts',(0.695205119431131,17.7481848420472,-15.8749999948272));
#26402=CARTESIAN_POINT('Ctrl Pts',(0.695207369782971,17.7481839415913,-15.8749999948272));
#26403=CARTESIAN_POINT('Ctrl Pts',(0.792820281938614,17.7091251069099,-15.8749999932568));
#26404=CARTESIAN_POINT('Ctrl Pts',(0.889818282082731,17.6685776890752,-15.8749999939569));
#26405=CARTESIAN_POINT('Ctrl Pts',(0.986075309087794,17.6263508819597,-15.874999995884));
#26406=CARTESIAN_POINT('Ctrl Pts',(1.0779093479489,17.5860643868717,-15.8749999977226));
#26407=CARTESIAN_POINT('Ctrl Pts',(1.16906840852933,17.544249418016,-15.8749999995905));
#26408=CARTESIAN_POINT('Ctrl Pts',(1.25946486042866,17.5007819756592,-15.8749999998948));
#26409=CARTESIAN_POINT('Ctrl Pts',(1.29635651290361,17.4830424986808,-15.875000000019));
#26410=CARTESIAN_POINT('Ctrl Pts',(1.33312145695237,17.4650282848733,-15.875));
#26411=CARTESIAN_POINT('Ctrl Pts',(1.36975523467035,17.4467329717171,-15.875));
#26412=CARTESIAN_POINT('Ctrl Pts',(1.36977642588146,17.4467223885923,-15.875));
#26413=CARTESIAN_POINT('Ctrl Pts',(1.36979761704848,17.4467118053719,-15.875));
#26414=CARTESIAN_POINT('Ctrl Pts',(1.36981880817139,17.4467012220559,-15.875));
#26415=CARTESIAN_POINT('Ctrl Pts',(1.48005617514885,17.3916462402392,-15.875));
#26416=CARTESIAN_POINT('Ctrl Pts',(1.58909781966939,17.3339013736985,-15.875));
#26417=CARTESIAN_POINT('Ctrl Pts',(1.69590260920769,17.2733228121837,-15.875));
#26418=CARTESIAN_POINT('Ctrl Pts',(1.80272792862359,17.2127326063367,-15.875));
#26419=CARTESIAN_POINT('Ctrl Pts',(1.90750675821464,17.1492444885504,-15.875));
#26420=CARTESIAN_POINT('Ctrl Pts',(2.00963535661709,17.0820035460311,-15.875));
#26421=CARTESIAN_POINT('Ctrl Pts',(2.00964517091121,17.0819970843505,-15.875));
#26422=CARTESIAN_POINT('Ctrl Pts',(2.00965498518143,17.0819906226361,-15.875));
#26423=CARTESIAN_POINT('Ctrl Pts',(2.00966479942777,17.0819841608878,-15.875));
#26424=CARTESIAN_POINT('Ctrl Pts',(2.11178308708155,17.014748975667,-15.875));
#26425=CARTESIAN_POINT('Ctrl Pts',(2.21131503888981,16.9438514389378,-15.875));
#26426=CARTESIAN_POINT('Ctrl Pts',(2.30688671952936,16.8673460056645,-15.875));
#26427=CARTESIAN_POINT('Ctrl Pts',(2.30689131206627,16.8673423293241,-15.875));
#26428=CARTESIAN_POINT('Ctrl Pts',(2.30689590459396,16.8673386529707,-15.875));
#26429=CARTESIAN_POINT('Ctrl Pts',(2.30690049711243,16.8673349766043,-15.875));
#26430=CARTESIAN_POINT('Ctrl Pts',(2.35469121108945,16.8290779335589,-15.875));
#26431=CARTESIAN_POINT('Ctrl Pts',(2.40147429518024,16.789416499467,-15.875));
#26432=CARTESIAN_POINT('Ctrl Pts',(2.4468278441479,16.7477195558332,-15.875));
#26433=CARTESIAN_POINT('Ctrl Pts',(2.49217613728494,16.7060274442816,-15.875));
#26434=CARTESIAN_POINT('Ctrl Pts',(2.53621611943434,16.6624266103822,-15.875));
#26435=CARTESIAN_POINT('Ctrl Pts',(2.57755123502764,16.6150404676675,-15.875));
#26436=CARTESIAN_POINT('Ctrl Pts',(2.57755123502976,16.6150404676651,-15.875));
#26437=CARTESIAN_POINT('Ctrl Pts',(3.09339220814419,16.0236857897033,-15.875));
#26438=CARTESIAN_POINT('Ctrl Pts',(3.62953325790838,15.452428023713,-15.875));
#26439=CARTESIAN_POINT('Ctrl Pts',(4.22657730609841,14.9414637355988,-15.875));
#26440=CARTESIAN_POINT('Ctrl Pts',(4.46002708929085,14.7416719402682,-15.875));
#26441=CARTESIAN_POINT('Ctrl Pts',(4.70080932940665,14.5526624071818,-15.875));
#26442=CARTESIAN_POINT('Ctrl Pts',(4.95042406413429,14.3770855263889,-15.875));
#26443=CARTESIAN_POINT('Ctrl Pts',(5.1714780269072,14.2215980496062,-15.875));
#26444=CARTESIAN_POINT('Ctrl Pts',(5.39945880318352,14.076644774025,-15.875));
#26445=CARTESIAN_POINT('Ctrl Pts',(5.63543015960283,13.9441001459419,-15.875));
#26446=CARTESIAN_POINT('Ctrl Pts',(5.81446516266139,13.8435365510449,-15.875));
#26447=CARTESIAN_POINT('Ctrl Pts',(5.99810030405848,13.7501165276488,-15.875));
#26448=CARTESIAN_POINT('Ctrl Pts',(6.18681074697913,13.6646760949928,-15.875));
#26449=CARTESIAN_POINT('Origin',(0.,0.,0.));
#26450=CARTESIAN_POINT('',(2.57755123502967,16.615040467665,0.));
#26451=CARTESIAN_POINT('Ctrl Pts',(6.18681074697836,13.6646760949931,-3.90312782094782E-15));
#26452=CARTESIAN_POINT('Ctrl Pts',(6.04942753363656,13.7268776390737,-3.90312782094782E-15));
#26453=CARTESIAN_POINT('Ctrl Pts',(5.91423497832213,13.7936520592212,-3.9031272724464E-15));
#26454=CARTESIAN_POINT('Ctrl Pts',(5.7813107133205,13.864489733245,-3.90312839779568E-15));
#26455=CARTESIAN_POINT('Ctrl Pts',(5.64040818592427,13.9395791633405,-3.90312959068968E-15));
#26456=CARTESIAN_POINT('Ctrl Pts',(5.50205371444,14.0192348081498,-3.90312762761502E-15));
#26457=CARTESIAN_POINT('Ctrl Pts',(5.36636167343317,14.1029047606296,-3.90316800608413E-15));
#26458=CARTESIAN_POINT('Ctrl Pts',(5.29440249028531,14.1472759808558,-3.90318941929032E-15));
#26459=CARTESIAN_POINT('Ctrl Pts',(5.22319249184617,14.1927770027392,-3.90322389755505E-15));
#26460=CARTESIAN_POINT('Ctrl Pts',(5.15275208328281,14.2393303034112,-3.90329226654004E-15));
#26461=CARTESIAN_POINT('Ctrl Pts',(4.82417650905236,14.4564823303883,-3.90361117977412E-15));
#26462=CARTESIAN_POINT('Ctrl Pts',(4.51455185467436,14.694538151671,-3.90293915145114E-15));
#26463=CARTESIAN_POINT('Ctrl Pts',(4.21891718821264,14.9480256152927,-3.90333349758813E-15));
#26464=CARTESIAN_POINT('Ctrl Pts',(3.62764785528921,15.4550005425363,-3.9041221898621E-15));
#26465=CARTESIAN_POINT('Ctrl Pts',(3.09286826794445,16.0242864292495,-3.9031278220838E-15));
#26466=CARTESIAN_POINT('Ctrl Pts',(2.57755123502973,16.6150404676649,-3.90312782094782E-15));
#26467=CARTESIAN_POINT('Ctrl Pts',(2.57755123502967,16.615040467665,-3.90312782094782E-15));
#26468=CARTESIAN_POINT('Ctrl Pts',(2.53664321583118,16.6619369915551,-3.90312783753E-15));
#26469=CARTESIAN_POINT('Ctrl Pts',(2.49260173716415,16.7056313191094,-4.86323593045554E-15));
#26470=CARTESIAN_POINT('Ctrl Pts',(2.44692282074809,16.7476322243581,-4.45426722229462E-15));
#26471=CARTESIAN_POINT('Ctrl Pts',(2.40124621644852,16.7896310036591,-4.04531921478443E-15));
#26472=CARTESIAN_POINT('Ctrl Pts',(2.35376064355281,16.8298668109454,-3.90316469176341E-15));
#26473=CARTESIAN_POINT('Ctrl Pts',(2.30550348248287,16.8684526549718,-3.90360339707742E-15));
#26474=CARTESIAN_POINT('Ctrl Pts',(2.30549795427634,16.868457075259,-3.90360344733428E-15));
#26475=CARTESIAN_POINT('Ctrl Pts',(2.30549242605973,16.8684614955246,-3.90360349758508E-15));
#26476=CARTESIAN_POINT('Ctrl Pts',(2.30548689783303,16.8684659157685,-3.90360354782982E-15));
#26477=CARTESIAN_POINT('Ctrl Pts',(2.20897530897574,16.9456343795253,-3.90448071870476E-15));
#26478=CARTESIAN_POINT('Ctrl Pts',(2.1088973161954,17.0167607154954,-3.80478103571114E-15));
#26479=CARTESIAN_POINT('Ctrl Pts',(2.00654625140481,17.0840357067547,-4.01874756173234E-15));
#26480=CARTESIAN_POINT('Ctrl Pts',(2.00653452597976,17.0840434138349,-4.01877207391958E-15));
#26481=CARTESIAN_POINT('Ctrl Pts',(2.00652280052487,17.0840511208646,-4.01879658554702E-15));
#26482=CARTESIAN_POINT('Ctrl Pts',(2.00651107504016,17.0840588278437,-4.0188210966111E-15));
#26483=CARTESIAN_POINT('Ctrl Pts',(1.90414776448742,17.1513406433296,-4.23280232840214E-15));
#26484=CARTESIAN_POINT('Ctrl Pts',(1.7994492991963,17.2146660834217,-4.13342344656728E-15));
#26485=CARTESIAN_POINT('Ctrl Pts',(1.6929747873709,17.274982420926,-4.03076142423713E-15));
#26486=CARTESIAN_POINT('Ctrl Pts',(1.58652466725004,17.3352849408672,-3.9281229202277E-15));
#26487=CARTESIAN_POINT('Ctrl Pts',(1.47828499287738,17.3925554738715,-3.90603445548038E-15));
#26488=CARTESIAN_POINT('Ctrl Pts',(1.36856924611844,17.4473251477231,-3.91849178334325E-15));
#26489=CARTESIAN_POINT('Ctrl Pts',(1.36854410497944,17.4473376980819,-3.91849463791446E-15));
#26490=CARTESIAN_POINT('Ctrl Pts',(1.36851896376299,17.4473502483093,-3.91849749145131E-15));
#26491=CARTESIAN_POINT('Ctrl Pts',(1.36849382246909,17.4473627984054,-3.91850034395322E-15));
#26492=CARTESIAN_POINT('Ctrl Pts',(1.14904840747076,17.5569061278786,-3.94339836500619E-15));
#26493=CARTESIAN_POINT('Ctrl Pts',(0.923340187830619,17.6566523551606,-3.89436736404263E-15));
#26494=CARTESIAN_POINT('Ctrl Pts',(0.694759689676839,17.7481734415667,-3.93289872637456E-15));
#26495=CARTESIAN_POINT('Ctrl Pts',(0.694723521974647,17.7481879227119,-3.93290482309256E-15));
#26496=CARTESIAN_POINT('Ctrl Pts',(0.694687354237592,17.7482024036388,-3.93292082649647E-15));
#26497=CARTESIAN_POINT('Ctrl Pts',(0.69465118646567,17.7482168843473,-3.93294675089361E-15));
#26498=CARTESIAN_POINT('Ctrl Pts',(0.500498710332174,17.8259508797229,-4.07211169335415E-15));
#26499=CARTESIAN_POINT('Ctrl Pts',(0.305013033138498,17.8973939584755,-2.1129514982979E-11));
#26500=CARTESIAN_POINT('Ctrl Pts',(0.106113584617659,17.9646283560373,-2.93212936336714E-12));
#26501=CARTESIAN_POINT('Ctrl Pts',(0.0708535797065735,17.9765473694174,
2.9382179480916E-13));
#26502=CARTESIAN_POINT('Ctrl Pts',(0.0354862560896116,17.9883340325599,
-3.35120567100207E-15));
#26503=CARTESIAN_POINT('Ctrl Pts',(1.34330150810747E-13,18.,-3.25260651745651E-15));
#26504=CARTESIAN_POINT('',(-2.57755123502756,16.6150404676675,0.));
#26505=CARTESIAN_POINT('Ctrl Pts',(1.00919272938427E-13,18.,-3.25260651745651E-15));
#26506=CARTESIAN_POINT('Ctrl Pts',(-0.163234977781181,17.9463369036664,
-3.70647810751983E-15));
#26507=CARTESIAN_POINT('Ctrl Pts',(-0.325479608497338,17.8896358852711,
-2.075071171567E-10));
#26508=CARTESIAN_POINT('Ctrl Pts',(-0.486261433812618,17.829207744229,-2.15138301120851E-9));
#26509=CARTESIAN_POINT('Ctrl Pts',(-0.556197159254499,17.8029231447565,
-2.9969162084646E-9));
#26510=CARTESIAN_POINT('Ctrl Pts',(-0.625856269235421,17.7759340381391,
-4.05715075919456E-9));
#26511=CARTESIAN_POINT('Ctrl Pts',(-0.69520061873086,17.748186642968,-5.17270802021755E-9));
#26512=CARTESIAN_POINT('Ctrl Pts',(-0.695202869082881,17.7481857425139,
-5.17274422210789E-9));
#26513=CARTESIAN_POINT('Ctrl Pts',(-0.695205119434567,17.748184842059,-5.17278042406062E-9));
#26514=CARTESIAN_POINT('Ctrl Pts',(-0.69520736978592,17.7481839416033,-5.17281662607575E-9));
#26515=CARTESIAN_POINT('Ctrl Pts',(-0.792820282116332,17.70912510685,-6.7431421330446E-9));
#26516=CARTESIAN_POINT('Ctrl Pts',(-0.889818282432727,17.6685776889372,
-6.04304683973043E-9));
#26517=CARTESIAN_POINT('Ctrl Pts',(-0.986075309607311,17.6263508817377,
-4.1159309985783E-9));
#26518=CARTESIAN_POINT('Ctrl Pts',(-1.07790934859941,17.586064386583,-2.27736568554749E-9));
#26519=CARTESIAN_POINT('Ctrl Pts',(-1.16906840930876,17.5442494176561,-4.09449895856158E-10));
#26520=CARTESIAN_POINT('Ctrl Pts',(-1.25946486133493,17.5007819752242,-1.0514569748843E-10));
#26521=CARTESIAN_POINT('Ctrl Pts',(-1.29635651350569,17.4830424983862,1.90437412412553E-11));
#26522=CARTESIAN_POINT('Ctrl Pts',(-1.33312145725236,17.4650282847238,-3.91465477576115E-15));
#26523=CARTESIAN_POINT('Ctrl Pts',(-1.36975523467049,17.4467329717176,-3.90420294014398E-15));
#26524=CARTESIAN_POINT('Ctrl Pts',(-1.36977642588111,17.446722388593,-3.90419689416495E-15));
#26525=CARTESIAN_POINT('Ctrl Pts',(-1.36979761704765,17.4467118053728,-3.90419380688497E-15));
#26526=CARTESIAN_POINT('Ctrl Pts',(-1.36981880817008,17.4467012220571,-3.90419364112946E-15));
#26527=CARTESIAN_POINT('Ctrl Pts',(-1.48005617514827,17.3916462402406,-3.90333137200445E-15));
#26528=CARTESIAN_POINT('Ctrl Pts',(-1.58909781966898,17.3339013736989,-3.90950951142143E-15));
#26529=CARTESIAN_POINT('Ctrl Pts',(-1.69590260920755,17.2733228121837,-3.97030686335835E-15));
#26530=CARTESIAN_POINT('Ctrl Pts',(-1.80272792862322,17.2127326063365,-4.03111590168284E-15));
#26531=CARTESIAN_POINT('Ctrl Pts',(-1.90750675821447,17.1492444885502,-4.090111775224E-15));
#26532=CARTESIAN_POINT('Ctrl Pts',(-2.00963535661692,17.082003546031,-3.9687347184938E-15));
#26533=CARTESIAN_POINT('Ctrl Pts',(-2.00964517091037,17.0819970843508,-3.96872305447342E-15));
#26534=CARTESIAN_POINT('Ctrl Pts',(-2.00965498517993,17.0819906226368,-3.96871139022941E-15));
#26535=CARTESIAN_POINT('Ctrl Pts',(-2.0096647994256,17.0819841608889,-3.96869972576296E-15));
#26536=CARTESIAN_POINT('Ctrl Pts',(-2.11178308708009,17.0147489756678,-3.84732969085294E-15));
#26537=CARTESIAN_POINT('Ctrl Pts',(-2.21131503888902,16.9438514389382,-3.91028333280058E-15));
#26538=CARTESIAN_POINT('Ctrl Pts',(-2.30688671952919,16.8673460056643,-3.90564247479998E-15));
#26539=CARTESIAN_POINT('Ctrl Pts',(-2.30689131206538,16.8673423293246,-3.90564225179136E-15));
#26540=CARTESIAN_POINT('Ctrl Pts',(-2.30689590459235,16.8673386529717,-3.90564202876022E-15));
#26541=CARTESIAN_POINT('Ctrl Pts',(-2.30690049711011,16.8673349766059,-3.90564180570655E-15));
#26542=CARTESIAN_POINT('Ctrl Pts',(-2.35469121108777,16.8290779335601,-3.90332066193792E-15));
#26543=CARTESIAN_POINT('Ctrl Pts',(-2.40147429518223,16.7894164994713,-4.08152894233206E-15));
#26544=CARTESIAN_POINT('Ctrl Pts',(-2.44682784415303,16.7477195558388,-4.56166899524867E-15));
#26545=CARTESIAN_POINT('Ctrl Pts',(-2.49217613729193,16.7060274442897,-5.04175340675553E-15));
#26546=CARTESIAN_POINT('Ctrl Pts',(-2.53621611943382,16.6624266103826,-3.90312784896662E-15));
#26547=CARTESIAN_POINT('Ctrl Pts',(-2.57755123502756,16.6150404676675,-3.90312782094782E-15));
#26548=CARTESIAN_POINT('Ctrl Pts',(-2.57755123502756,16.6150404676675,-3.90312782094782E-15));
#26549=CARTESIAN_POINT('Ctrl Pts',(-3.09339220814233,16.0236857897052,-3.90312781973625E-15));
#26550=CARTESIAN_POINT('Ctrl Pts',(-3.62953325790676,15.4524280237144,-3.90460918672713E-15));
#26551=CARTESIAN_POINT('Ctrl Pts',(-4.22657730609724,14.9414637356001,-3.90365083757559E-15));
#26552=CARTESIAN_POINT('Ctrl Pts',(-4.46002708931194,14.7416719402505,-3.90327611413184E-15));
#26553=CARTESIAN_POINT('Ctrl Pts',(-4.70080932945974,14.5526624071656,-3.96947826803498E-15));
#26554=CARTESIAN_POINT('Ctrl Pts',(-4.95042406421973,14.3770855263738,-4.05016361199005E-15));
#26555=CARTESIAN_POINT('Ctrl Pts',(-5.17147802720282,14.2215980494645,-4.12161698613911E-15));
#26556=CARTESIAN_POINT('Ctrl Pts',(-5.39945880370098,14.0766447737736,-4.20445864407361E-15));
#26557=CARTESIAN_POINT('Ctrl Pts',(-5.63543016034986,13.9441001455877,-4.26266359505368E-15));
#26558=CARTESIAN_POINT('Ctrl Pts',(-5.81446516317737,13.8435365508404,-4.30682456319525E-15));
#26559=CARTESIAN_POINT('Ctrl Pts',(-5.99810030432704,13.7501165275657,-4.33680868994202E-15));
#26560=CARTESIAN_POINT('Ctrl Pts',(-6.18681074697897,13.6646760949927,-4.33680868994202E-15));
#26561=CARTESIAN_POINT('Origin',(0.,76.,-7.93749999999999));
#26562=CARTESIAN_POINT('Origin',(4.32565866516615,20.8014139268345,-1.69615259943912));
#26563=CARTESIAN_POINT('',(3.73830603269933,20.2061012558294,-2.5436239488228));
#26564=CARTESIAN_POINT('',(4.52144288428828,20.9998514259673,-1.41366213459292));
#26565=CARTESIAN_POINT('',(3.7383057650626,19.5711013646158,-2.543623843377));
#26566=CARTESIAN_POINT('',(3.73830577451205,19.5711012915154,-2.54362383229417));
#26567=CARTESIAN_POINT('',(3.73830600779846,20.2061009926513,-2.54362399397926));
#26568=CARTESIAN_POINT('Ctrl Pts',(-6.56268467749999,75.2062500034686,-7.93749999999999));
#26569=CARTESIAN_POINT('Ctrl Pts',(-6.56268467749997,75.0792500034686,-10.0698455118856));
#26570=CARTESIAN_POINT('Ctrl Pts',(-5.30932343282159,74.9522500034687,-11.7949492688802));
#26571=CARTESIAN_POINT('Ctrl Pts',(-4.05596218814312,74.8252500034686,-13.5200530258749));
#26572=CARTESIAN_POINT('Ctrl Pts',(-2.0279810940716,74.6982500034687,-14.1789840269267));
#26573=CARTESIAN_POINT('Ctrl Pts',(0.,74.5712500034686,-14.8379150279786));
#26574=CARTESIAN_POINT('Ctrl Pts',(2.0279810940716,74.4442500034688,-14.1789840269267));
#26575=CARTESIAN_POINT('Ctrl Pts',(4.05596218814312,74.3172500034686,-13.5200530258749));
#26576=CARTESIAN_POINT('Ctrl Pts',(5.30932343282159,74.1902500034686,-11.7949492688802));
#26577=CARTESIAN_POINT('Ctrl Pts',(6.56268467750008,74.0632500034686,-10.0698455118856));
#26578=CARTESIAN_POINT('Ctrl Pts',(6.5626846775001,73.9362500034686,-7.93749999999999));
#26579=CARTESIAN_POINT('Ctrl Pts',(6.56268467749991,73.8092500034686,-5.80515448811441));
#26580=CARTESIAN_POINT('Ctrl Pts',(5.30932343282159,73.6822500034686,-4.08005073111967));
#26581=CARTESIAN_POINT('Ctrl Pts',(4.05596218814324,73.5552500034685,-2.35494697412514));
#26582=CARTESIAN_POINT('Ctrl Pts',(2.02798109407165,73.4282500034686,-1.69601597307328));
#26583=CARTESIAN_POINT('Ctrl Pts',(0.,73.3012500034685,-1.0370849720215));
#26584=CARTESIAN_POINT('Ctrl Pts',(-2.02798109407154,73.1742500034685,-1.69601597307328));
#26585=CARTESIAN_POINT('Ctrl Pts',(-4.05596218814312,73.0472500034686,-2.35494697412514));
#26586=CARTESIAN_POINT('Ctrl Pts',(-5.30932343282159,72.9202500034686,-4.08005073111967));
#26587=CARTESIAN_POINT('Ctrl Pts',(-6.56268467750003,72.7932500034685,-5.80515448811441));
#26588=CARTESIAN_POINT('Ctrl Pts',(-6.56268467749993,72.6662500034687,-7.93749999999999));
#26589=CARTESIAN_POINT('Ctrl Pts',(-6.56268467749997,72.5392500034685,-10.0698455118856));
#26590=CARTESIAN_POINT('Ctrl Pts',(-5.30932343282159,72.4122500034687,-11.7949492688802));
#26591=CARTESIAN_POINT('Ctrl Pts',(-4.05596218814312,72.2852500034686,-13.5200530258749));
#26592=CARTESIAN_POINT('Ctrl Pts',(-2.0279810940716,72.1582500034688,-14.1789840269267));
#26593=CARTESIAN_POINT('Ctrl Pts',(0.,72.0312500034686,-14.8379150279786));
#26594=CARTESIAN_POINT('Ctrl Pts',(2.02798109407154,71.9042500034687,-14.1789840269267));
#26595=CARTESIAN_POINT('Ctrl Pts',(4.05596218814318,71.7772500034686,-13.5200530258749));
#26596=CARTESIAN_POINT('Ctrl Pts',(5.30932343282159,71.6502500034686,-11.7949492688802));
#26597=CARTESIAN_POINT('Ctrl Pts',(6.56268467750003,71.5232500034685,-10.0698455118856));
#26598=CARTESIAN_POINT('Ctrl Pts',(6.5626846775001,71.3962500034686,-7.93749999999999));
#26599=CARTESIAN_POINT('Ctrl Pts',(6.56268467750008,71.2692500034686,-5.80515448811441));
#26600=CARTESIAN_POINT('Ctrl Pts',(5.30932343282153,71.1422500034686,-4.08005073111967));
#26601=CARTESIAN_POINT('Ctrl Pts',(4.05596218814312,71.0152500034686,-2.35494697412514));
#26602=CARTESIAN_POINT('Ctrl Pts',(2.0279810940716,70.8882500034687,-1.69601597307328));
#26603=CARTESIAN_POINT('Ctrl Pts',(0.,70.7612500034686,-1.0370849720215));
#26604=CARTESIAN_POINT('Ctrl Pts',(-2.02798109407148,70.6342500034686,-1.69601597307328));
#26605=CARTESIAN_POINT('Ctrl Pts',(-4.05596218814318,70.5072500034686,-2.35494697412514));
#26606=CARTESIAN_POINT('Ctrl Pts',(-5.30932343282159,70.3802500034686,-4.08005073111967));
#26607=CARTESIAN_POINT('Ctrl Pts',(-6.56268467750003,70.2532500034686,-5.80515448811441));
#26608=CARTESIAN_POINT('Ctrl Pts',(-6.56268467749999,70.1262500034686,-7.93749999999999));
#26609=CARTESIAN_POINT('Ctrl Pts',(-6.56268467750003,69.9992500034686,-10.0698455118856));
#26610=CARTESIAN_POINT('Ctrl Pts',(-5.30932343282153,69.8722500034687,-11.7949492688802));
#26611=CARTESIAN_POINT('Ctrl Pts',(-4.05596218814324,69.7452500034685,-13.5200530258749));
#26612=CARTESIAN_POINT('Ctrl Pts',(-2.02798109407154,69.6182500034687,-14.1789840269267));
#26613=CARTESIAN_POINT('Ctrl Pts',(-5.83678785436452E-14,69.4912500034686,
-14.8379150279786));
#26614=CARTESIAN_POINT('Ctrl Pts',(2.02798109407154,69.3642500034687,-14.1789840269267));
#26615=CARTESIAN_POINT('Ctrl Pts',(4.05596218814318,69.2372500034687,-13.5200530258749));
#26616=CARTESIAN_POINT('Ctrl Pts',(5.30932343282164,69.1102500034686,-11.7949492688802));
#26617=CARTESIAN_POINT('Ctrl Pts',(6.56268467750003,68.9832500034685,-10.0698455118856));
#26618=CARTESIAN_POINT('Ctrl Pts',(6.56268467749999,68.8562500034686,-7.93749999999999));
#26619=CARTESIAN_POINT('Ctrl Pts',(6.56268467750003,68.7292500034685,-5.80515448811441));
#26620=CARTESIAN_POINT('Ctrl Pts',(5.30932343282159,68.6022500034686,-4.08005073111967));
#26621=CARTESIAN_POINT('Ctrl Pts',(4.05596218814318,68.4752500034685,-2.35494697412514));
#26622=CARTESIAN_POINT('Ctrl Pts',(2.0279810940716,68.3482500034686,-1.69601597307328));
#26623=CARTESIAN_POINT('Ctrl Pts',(-1.1673575708729E-13,68.2212500034685,
-1.0370849720215));
#26624=CARTESIAN_POINT('Ctrl Pts',(-2.02798109407154,68.0942500034687,-1.69601597307328));
#26625=CARTESIAN_POINT('Ctrl Pts',(-4.05596218814306,67.9672500034686,-2.35494697412514));
#26626=CARTESIAN_POINT('Ctrl Pts',(-5.30932343282159,67.8402500034686,-4.08005073111967));
#26627=CARTESIAN_POINT('Ctrl Pts',(-6.56268467749997,67.7132500034685,-5.80515448811441));
#26628=CARTESIAN_POINT('Ctrl Pts',(-6.56268467749999,67.5862500034686,-7.93749999999999));
#26629=CARTESIAN_POINT('Ctrl Pts',(-6.56268467749991,67.4592500034685,-10.0698455118856));
#26630=CARTESIAN_POINT('Ctrl Pts',(-5.30932343282153,67.3322500034686,-11.7949492688802));
#26631=CARTESIAN_POINT('Ctrl Pts',(-4.05596218814312,67.2052500034686,-13.5200530258749));
#26632=CARTESIAN_POINT('Ctrl Pts',(-2.02798109407154,67.0782500034687,-14.1789840269267));
#26633=CARTESIAN_POINT('Ctrl Pts',(0.,66.9512500034685,-14.8379150279786));
#26634=CARTESIAN_POINT('Ctrl Pts',(2.02798109407154,66.8242500034687,-14.1789840269267));
#26635=CARTESIAN_POINT('Ctrl Pts',(4.05596218814318,66.6972500034686,-13.5200530258749));
#26636=CARTESIAN_POINT('Ctrl Pts',(5.30932343282153,66.5702500034686,-11.7949492688802));
#26637=CARTESIAN_POINT('Ctrl Pts',(6.56268467750003,66.4432500034685,-10.0698455118856));
#26638=CARTESIAN_POINT('Ctrl Pts',(6.56268467749999,66.3162500034687,-7.93749999999999));
#26639=CARTESIAN_POINT('Ctrl Pts',(6.56268467749997,66.1892500034686,-5.80515448811441));
#26640=CARTESIAN_POINT('Ctrl Pts',(5.30932343282159,66.0622500034686,-4.08005073111967));
#26641=CARTESIAN_POINT('Ctrl Pts',(4.05596218814318,65.9352500034686,-2.35494697412514));
#26642=CARTESIAN_POINT('Ctrl Pts',(2.02798109407148,65.8082500034686,-1.69601597307328));
#26643=CARTESIAN_POINT('Ctrl Pts',(5.83678785436452E-14,65.6812500034686,
-1.0370849720215));
#26644=CARTESIAN_POINT('Ctrl Pts',(-2.0279810940716,65.5542500034686,-1.69601597307328));
#26645=CARTESIAN_POINT('Ctrl Pts',(-4.05596218814318,65.4272500034686,-2.35494697412514));
#26646=CARTESIAN_POINT('Ctrl Pts',(-5.30932343282153,65.3002500034686,-4.08005073111967));
#26647=CARTESIAN_POINT('Ctrl Pts',(-6.56268467749997,65.1732500034685,-5.80515448811441));
#26648=CARTESIAN_POINT('Ctrl Pts',(-6.56268467749999,65.0462500034685,-7.93749999999999));
#26649=CARTESIAN_POINT('Ctrl Pts',(-6.56268467750003,64.9192500034685,-10.0698455118856));
#26650=CARTESIAN_POINT('Ctrl Pts',(-5.30932343282159,64.7922500034686,-11.7949492688802));
#26651=CARTESIAN_POINT('Ctrl Pts',(-4.05596218814306,64.6652500034686,-13.5200530258749));
#26652=CARTESIAN_POINT('Ctrl Pts',(-2.02798109407154,64.5382500034687,-14.1789840269267));
#26653=CARTESIAN_POINT('Ctrl Pts',(1.1673575708729E-13,64.4112500034686,
-14.8379150279786));
#26654=CARTESIAN_POINT('Ctrl Pts',(2.0279810940716,64.2842500034687,-14.1789840269267));
#26655=CARTESIAN_POINT('Ctrl Pts',(4.05596218814324,64.1572500034685,-13.5200530258749));
#26656=CARTESIAN_POINT('Ctrl Pts',(5.30932343282159,64.0302500034686,-11.7949492688802));
#26657=CARTESIAN_POINT('Ctrl Pts',(6.56268467750003,63.9032500034685,-10.0698455118856));
#26658=CARTESIAN_POINT('Ctrl Pts',(6.56268467749999,63.7762500034686,-7.93749999999999));
#26659=CARTESIAN_POINT('Ctrl Pts',(6.56268467750008,63.6492500034686,-5.80515448811441));
#26660=CARTESIAN_POINT('Ctrl Pts',(5.30932343282159,63.5222500034686,-4.08005073111967));
#26661=CARTESIAN_POINT('Ctrl Pts',(4.05596218814318,63.3952500034686,-2.35494697412514));
#26662=CARTESIAN_POINT('Ctrl Pts',(2.02798109407154,63.2682500034685,-1.69601597307328));
#26663=CARTESIAN_POINT('Ctrl Pts',(0.,63.1412500034685,-1.0370849720215));
#26664=CARTESIAN_POINT('Ctrl Pts',(-2.02798109407154,63.0142500034686,-1.69601597307328));
#26665=CARTESIAN_POINT('Ctrl Pts',(-4.05596218814318,62.8872500034686,-2.35494697412514));
#26666=CARTESIAN_POINT('Ctrl Pts',(-5.30932343282164,62.7602500034687,-4.08005073111967));
#26667=CARTESIAN_POINT('Ctrl Pts',(-6.56268467749997,62.6332500034685,-5.80515448811441));
#26668=CARTESIAN_POINT('Ctrl Pts',(-6.56268467749999,62.5062500034685,-7.93749999999999));
#26669=CARTESIAN_POINT('Ctrl Pts',(-6.56268467750003,62.3792500034687,-10.0698455118856));
#26670=CARTESIAN_POINT('Ctrl Pts',(-5.30932343282159,62.2522500034686,-11.7949492688802));
#26671=CARTESIAN_POINT('Ctrl Pts',(-4.05596218814318,62.1252500034685,-13.5200530258749));
#26672=CARTESIAN_POINT('Ctrl Pts',(-2.02798109407148,61.9982500034687,-14.1789840269267));
#26673=CARTESIAN_POINT('Ctrl Pts',(0.,61.8712500034686,-14.8379150279786));
#26674=CARTESIAN_POINT('Ctrl Pts',(2.0279810940716,61.7442500034687,-14.1789840269267));
#26675=CARTESIAN_POINT('Ctrl Pts',(4.05596218814312,61.6172500034686,-13.5200530258749));
#26676=CARTESIAN_POINT('Ctrl Pts',(5.30932343282159,61.4902500034686,-11.7949492688802));
#26677=CARTESIAN_POINT('Ctrl Pts',(6.56268467749991,61.3632500034686,-10.0698455118856));
#26678=CARTESIAN_POINT('Ctrl Pts',(6.56268467749993,61.2362500034686,-7.93749999999999));
#26679=CARTESIAN_POINT('Ctrl Pts',(6.56268467750003,61.1092500034686,-5.80515448811441));
#26680=CARTESIAN_POINT('Ctrl Pts',(5.30932343282159,60.9822500034687,-4.08005073111967));
#26681=CARTESIAN_POINT('Ctrl Pts',(4.05596218814306,60.8552500034686,-2.35494697412514));
#26682=CARTESIAN_POINT('Ctrl Pts',(2.02798109407154,60.7282500034685,-1.69601597307328));
#26683=CARTESIAN_POINT('Ctrl Pts',(0.,60.6012500034686,-1.0370849720215));
#26684=CARTESIAN_POINT('Ctrl Pts',(-2.02798109407154,60.4742500034686,-1.69601597307317));
#26685=CARTESIAN_POINT('Ctrl Pts',(-4.05596218814312,60.3472500034685,-2.35494697412514));
#26686=CARTESIAN_POINT('Ctrl Pts',(-5.30932343282159,60.2202500034686,-4.08005073111967));
#26687=CARTESIAN_POINT('Ctrl Pts',(-6.56268467749997,60.0932500034686,-5.80515448811441));
#26688=CARTESIAN_POINT('Ctrl Pts',(-6.56268467749999,59.9662500034687,-7.93749999999999));
#26689=CARTESIAN_POINT('Ctrl Pts',(-6.56268467750003,59.8392500034686,-10.0698455118856));
#26690=CARTESIAN_POINT('Ctrl Pts',(-5.30932343282159,59.7122500034685,-11.7949492688802));
#26691=CARTESIAN_POINT('Ctrl Pts',(-4.05596218814306,59.5852500034686,-13.5200530258749));
#26692=CARTESIAN_POINT('Ctrl Pts',(-2.02798109407148,59.4582500034687,-14.1789840269267));
#26693=CARTESIAN_POINT('Ctrl Pts',(1.1673575708729E-13,59.3312500034686,
-14.8379150279786));
#26694=CARTESIAN_POINT('Ctrl Pts',(2.02798109407148,59.2042500034687,-14.1789840269267));
#26695=CARTESIAN_POINT('Ctrl Pts',(4.05596218814324,59.0772500034685,-13.5200530258749));
#26696=CARTESIAN_POINT('Ctrl Pts',(5.30932343282159,58.9502500034686,-11.7949492688802));
#26697=CARTESIAN_POINT('Ctrl Pts',(6.56268467750008,58.8232500034686,-10.0698455118856));
#26698=CARTESIAN_POINT('Ctrl Pts',(6.56268467749999,58.6962500034686,-7.93749999999999));
#26699=CARTESIAN_POINT('Ctrl Pts',(6.56268467750003,58.5692500034686,-5.80515448811441));
#26700=CARTESIAN_POINT('Ctrl Pts',(5.30932343282159,58.4422500034686,-4.08005073111967));
#26701=CARTESIAN_POINT('Ctrl Pts',(4.05596218814312,58.3152500034686,-2.35494697412514));
#26702=CARTESIAN_POINT('Ctrl Pts',(2.02798109407154,58.1882500034687,-1.69601597307328));
#26703=CARTESIAN_POINT('Ctrl Pts',(5.83678785436452E-14,58.0612500034686,
-1.0370849720215));
#26704=CARTESIAN_POINT('Ctrl Pts',(-2.02798109407154,57.9342500034686,-1.69601597307317));
#26705=CARTESIAN_POINT('Ctrl Pts',(-4.05596218814312,57.8072500034686,-2.35494697412514));
#26706=CARTESIAN_POINT('Ctrl Pts',(-5.30932343282159,57.6802500034686,-4.08005073111967));
#26707=CARTESIAN_POINT('Ctrl Pts',(-6.56268467750003,57.5532500034687,-5.80515448811441));
#26708=CARTESIAN_POINT('Ctrl Pts',(-6.56268467749993,57.4262500034687,-7.93749999999999));
#26709=CARTESIAN_POINT('Ctrl Pts',(-6.56268467749997,57.2992500034685,-10.0698455118856));
#26710=CARTESIAN_POINT('Ctrl Pts',(-5.30932343282159,57.1722500034686,-11.7949492688802));
#26711=CARTESIAN_POINT('Ctrl Pts',(-4.05596218814312,57.0452500034685,-13.5200530258749));
#26712=CARTESIAN_POINT('Ctrl Pts',(-2.0279810940716,56.9182500034687,-14.1789840269267));
#26713=CARTESIAN_POINT('Ctrl Pts',(0.,56.7912500034686,-14.8379150279786));
#26714=CARTESIAN_POINT('Ctrl Pts',(2.02798109407154,56.6642500034688,-14.1789840269267));
#26715=CARTESIAN_POINT('Ctrl Pts',(4.05596218814312,56.5372500034686,-13.5200530258749));
#26716=CARTESIAN_POINT('Ctrl Pts',(5.30932343282159,56.4102500034686,-11.7949492688802));
#26717=CARTESIAN_POINT('Ctrl Pts',(6.56268467750008,56.2832500034686,-10.0698455118856));
#26718=CARTESIAN_POINT('Ctrl Pts',(6.56268467749999,56.1562500034686,-7.93749999999999));
#26719=CARTESIAN_POINT('Ctrl Pts',(6.56268467750003,56.0292500034686,-5.80515448811441));
#26720=CARTESIAN_POINT('Ctrl Pts',(5.30932343282164,55.9022500034686,-4.08005073111967));
#26721=CARTESIAN_POINT('Ctrl Pts',(4.05596218814324,55.7752500034686,-2.35494697412514));
#26722=CARTESIAN_POINT('Ctrl Pts',(2.0279810940716,55.6482500034686,-1.69601597307317));
#26723=CARTESIAN_POINT('Ctrl Pts',(0.,55.5212500034686,-1.0370849720215));
#26724=CARTESIAN_POINT('Ctrl Pts',(-2.02798109407148,55.3942500034686,-1.69601597307317));
#26725=CARTESIAN_POINT('Ctrl Pts',(-4.05596218814312,55.2672500034686,-2.35494697412514));
#26726=CARTESIAN_POINT('Ctrl Pts',(-5.30932343282159,55.1402500034686,-4.08005073111967));
#26727=CARTESIAN_POINT('Ctrl Pts',(-6.56268467749991,55.0132500034686,-5.80515448811441));
#26728=CARTESIAN_POINT('Ctrl Pts',(-6.56268467749987,54.8862500034686,-7.93750000000004));
#26729=CARTESIAN_POINT('Ctrl Pts',(-6.56268467749997,54.7592500034686,-10.0698455118856));
#26730=CARTESIAN_POINT('Ctrl Pts',(-5.30932343282153,54.6322500034687,-11.7949492688803));
#26731=CARTESIAN_POINT('Ctrl Pts',(-4.05596218814312,54.5052500034686,-13.5200530258749));
#26732=CARTESIAN_POINT('Ctrl Pts',(-2.02798109407154,54.3782500034687,-14.1789840269267));
#26733=CARTESIAN_POINT('Ctrl Pts',(0.,54.2512500034685,-14.8379150279786));
#26734=CARTESIAN_POINT('Ctrl Pts',(2.02798109407154,54.1242500034687,-14.1789840269267));
#26735=CARTESIAN_POINT('Ctrl Pts',(4.05596218814312,53.9972500034686,-13.5200530258749));
#26736=CARTESIAN_POINT('Ctrl Pts',(5.30932343282164,53.8702500034687,-11.7949492688803));
#26737=CARTESIAN_POINT('Ctrl Pts',(6.56268467749997,53.7432500034685,-10.0698455118856));
#26738=CARTESIAN_POINT('Ctrl Pts',(6.56268467749999,53.6162500034686,-7.93750000000004));
#26739=CARTESIAN_POINT('Ctrl Pts',(6.56268467750003,53.4892500034685,-5.80515448811441));
#26740=CARTESIAN_POINT('Ctrl Pts',(5.30932343282159,53.3622500034686,-4.08005073111972));
#26741=CARTESIAN_POINT('Ctrl Pts',(4.05596218814312,53.2352500034685,-2.35494697412514));
#26742=CARTESIAN_POINT('Ctrl Pts',(2.0279810940716,53.1082500034686,-1.69601597307323));
#26743=CARTESIAN_POINT('Ctrl Pts',(0.,52.9812500034685,-1.0370849720215));
#26744=CARTESIAN_POINT('Ctrl Pts',(-2.02798109407148,52.8542500034686,-1.69601597307323));
#26745=CARTESIAN_POINT('Ctrl Pts',(-4.05596218814312,52.7272500034686,-2.35494697412514));
#26746=CARTESIAN_POINT('Ctrl Pts',(-5.30932343282159,52.6002500034685,-4.08005073111972));
#26747=CARTESIAN_POINT('Ctrl Pts',(-6.56268467750003,52.4732500034686,-5.80515448811441));
#26748=CARTESIAN_POINT('Ctrl Pts',(-6.56268467749999,52.3462500034686,-7.93750000000004));
#26749=CARTESIAN_POINT('Ctrl Pts',(-6.56268467749997,52.2192500034685,-10.0698455118856));
#26750=CARTESIAN_POINT('Ctrl Pts',(-5.30932343282153,52.0922500034686,-11.7949492688803));
#26751=CARTESIAN_POINT('Ctrl Pts',(-4.05596218814312,51.9652500034685,-13.5200530258749));
#26752=CARTESIAN_POINT('Ctrl Pts',(-2.02798109407154,51.8382500034687,-14.1789840269267));
#26753=CARTESIAN_POINT('Ctrl Pts',(0.,51.7112500034685,-14.8379150279786));
#26754=CARTESIAN_POINT('Ctrl Pts',(2.02798109407154,51.5842500034687,-14.1789840269267));
#26755=CARTESIAN_POINT('Ctrl Pts',(4.05596218814312,51.4572500034686,-13.5200530258749));
#26756=CARTESIAN_POINT('Ctrl Pts',(5.30932343282164,51.3302500034686,-11.7949492688803));
#26757=CARTESIAN_POINT('Ctrl Pts',(6.56268467750008,51.2032500034686,-10.0698455118856));
#26758=CARTESIAN_POINT('Ctrl Pts',(6.56268467749999,51.0762500034687,-7.93750000000004));
#26759=CARTESIAN_POINT('Ctrl Pts',(6.56268467749997,50.9492500034685,-5.80515448811441));
#26760=CARTESIAN_POINT('Ctrl Pts',(5.30932343282159,50.8222500034686,-4.08005073111972));
#26761=CARTESIAN_POINT('Ctrl Pts',(4.05596218814312,50.6952500034686,-2.35494697412514));
#26762=CARTESIAN_POINT('Ctrl Pts',(2.0279810940716,50.5682500034686,-1.69601597307323));
#26763=CARTESIAN_POINT('Ctrl Pts',(0.,50.4412500034686,-1.0370849720215));
#26764=CARTESIAN_POINT('Ctrl Pts',(-2.0279810940716,50.3142500034687,-1.69601597307323));
#26765=CARTESIAN_POINT('Ctrl Pts',(-4.05596218814312,50.1872500034686,-2.35494697412514));
#26766=CARTESIAN_POINT('Ctrl Pts',(-5.30932343282153,50.0602500034686,-4.08005073111972));
#26767=CARTESIAN_POINT('Ctrl Pts',(-6.56268467750003,49.9332500034686,-5.80515448811441));
#26768=CARTESIAN_POINT('Ctrl Pts',(-6.56268467749999,49.8062500034686,-7.93750000000004));
#26769=CARTESIAN_POINT('Ctrl Pts',(-6.56268467749997,49.6792500034685,-10.0698455118856));
#26770=CARTESIAN_POINT('Ctrl Pts',(-5.30932343282159,49.5522500034686,-11.7949492688803));
#26771=CARTESIAN_POINT('Ctrl Pts',(-4.05596218814312,49.4252500034686,-13.5200530258749));
#26772=CARTESIAN_POINT('Ctrl Pts',(-2.02798109407154,49.2982500034686,-14.1789840269267));
#26773=CARTESIAN_POINT('Ctrl Pts',(0.,49.1712500034685,-14.8379150279786));
#26774=CARTESIAN_POINT('Ctrl Pts',(2.0279810940716,49.0442500034687,-14.1789840269267));
#26775=CARTESIAN_POINT('Ctrl Pts',(4.05596218814318,48.9172500034685,-13.5200530258749));
#26776=CARTESIAN_POINT('Ctrl Pts',(5.30932343282159,48.7902500034686,-11.7949492688803));
#26777=CARTESIAN_POINT('Ctrl Pts',(6.56268467750003,48.6632500034685,-10.0698455118856));
#26778=CARTESIAN_POINT('Ctrl Pts',(6.56268467750004,48.5362500034686,-7.93750000000004));
#26779=CARTESIAN_POINT('Ctrl Pts',(6.56268467750008,48.4092500034685,-5.80515448811441));
#26780=CARTESIAN_POINT('Ctrl Pts',(5.30932343282159,48.2822500034686,-4.08005073111972));
#26781=CARTESIAN_POINT('Ctrl Pts',(4.05596218814312,48.1552500034686,-2.35494697412514));
#26782=CARTESIAN_POINT('Ctrl Pts',(2.02798109407154,48.0282500034685,-1.69601597307323));
#26783=CARTESIAN_POINT('Ctrl Pts',(0.,47.9012500034685,-1.0370849720215));
#26784=CARTESIAN_POINT('Ctrl Pts',(-2.02798109407154,47.7742500034686,-1.69601597307323));
#26785=CARTESIAN_POINT('Ctrl Pts',(-4.05596218814318,47.6472500034685,-2.35494697412514));
#26786=CARTESIAN_POINT('Ctrl Pts',(-5.30932343282153,47.5202500034686,-4.08005073111972));
#26787=CARTESIAN_POINT('Ctrl Pts',(-6.56268467750003,47.3932500034686,-5.80515448811441));
#26788=CARTESIAN_POINT('Ctrl Pts',(-6.56268467749999,47.2662500034685,-7.93750000000004));
#26789=CARTESIAN_POINT('Ctrl Pts',(-6.56268467750003,47.1392500034685,-10.0698455118856));
#26790=CARTESIAN_POINT('Ctrl Pts',(-5.30932343282159,47.0122500034686,-11.7949492688803));
#26791=CARTESIAN_POINT('Ctrl Pts',(-4.05596218814324,46.8852500034686,-13.5200530258749));
#26792=CARTESIAN_POINT('Ctrl Pts',(-2.02798109407148,46.7582500034687,-14.1789840269267));
#26793=CARTESIAN_POINT('Ctrl Pts',(-1.1673575708729E-13,46.6312500034685,
-14.8379150279786));
#26794=CARTESIAN_POINT('Ctrl Pts',(2.0279810940716,46.5042500034687,-14.1789840269267));
#26795=CARTESIAN_POINT('Ctrl Pts',(4.05596218814318,46.3772500034685,-13.5200530258749));
#26796=CARTESIAN_POINT('Ctrl Pts',(5.30932343282159,46.2502500034686,-11.7949492688803));
#26797=CARTESIAN_POINT('Ctrl Pts',(6.56268467750003,46.1232500034686,-10.0698455118856));
#26798=CARTESIAN_POINT('Ctrl Pts',(6.56268467749993,45.9962500034686,-7.93750000000004));
#26799=CARTESIAN_POINT('Ctrl Pts',(6.56268467750008,45.8692500034686,-5.80515448811441));
#26800=CARTESIAN_POINT('Ctrl Pts',(5.30932343282159,45.7422500034685,-4.08005073111972));
#26801=CARTESIAN_POINT('Ctrl Pts',(4.05596218814318,45.6152500034686,-2.35494697412514));
#26802=CARTESIAN_POINT('Ctrl Pts',(2.02798109407154,45.4882500034685,-1.69601597307323));
#26803=CARTESIAN_POINT('Ctrl Pts',(-1.1673575708729E-13,45.3612500034685,
-1.0370849720215));
#26804=CARTESIAN_POINT('Ctrl Pts',(-2.02798109407154,45.2342500034686,-1.69601597307323));
#26805=CARTESIAN_POINT('Ctrl Pts',(-4.05596218814306,45.1072500034685,-2.35494697412514));
#26806=CARTESIAN_POINT('Ctrl Pts',(-5.30932343282159,44.9802500034686,-4.08005073111972));
#26807=CARTESIAN_POINT('Ctrl Pts',(-6.56268467749997,44.8532500034685,-5.80515448811441));
#26808=CARTESIAN_POINT('Ctrl Pts',(-6.56268467749993,44.7262500034686,-7.93750000000004));
#26809=CARTESIAN_POINT('Ctrl Pts',(-6.56268467749991,44.5992500034686,-10.0698455118856));
#26810=CARTESIAN_POINT('Ctrl Pts',(-5.30932343282159,44.4722500034685,-11.7949492688803));
#26811=CARTESIAN_POINT('Ctrl Pts',(-4.05596218814306,44.3452500034686,-13.5200530258749));
#26812=CARTESIAN_POINT('Ctrl Pts',(-2.02798109407148,44.2182500034687,-14.1789840269267));
#26813=CARTESIAN_POINT('Ctrl Pts',(0.,44.0912500034687,-14.8379150279786));
#26814=CARTESIAN_POINT('Ctrl Pts',(2.0279810940716,43.9642500034687,-14.1789840269267));
#26815=CARTESIAN_POINT('Ctrl Pts',(4.05596218814318,43.8372500034685,-13.5200530258749));
#26816=CARTESIAN_POINT('Ctrl Pts',(5.30932343282159,43.7102500034686,-11.7949492688803));
#26817=CARTESIAN_POINT('Ctrl Pts',(6.56268467750003,43.5832500034686,-10.0698455118856));
#26818=CARTESIAN_POINT('Ctrl Pts',(6.56268467749999,43.4562500034686,-7.93750000000004));
#26819=CARTESIAN_POINT('Ctrl Pts',(6.56268467749997,43.3292500034686,-5.80515448811441));
#26820=CARTESIAN_POINT('Ctrl Pts',(5.30932343282164,43.2022500034686,-4.08005073111972));
#26821=CARTESIAN_POINT('Ctrl Pts',(4.05596218814306,43.0752500034686,-2.35494697412514));
#26822=CARTESIAN_POINT('Ctrl Pts',(2.02798109407154,42.9482500034687,-1.69601597307323));
#26823=CARTESIAN_POINT('Ctrl Pts',(1.1673575708729E-13,42.8212500034686,
-1.0370849720215));
#26824=CARTESIAN_POINT('Ctrl Pts',(-2.02798109407154,42.6942500034686,-1.69601597307323));
#26825=CARTESIAN_POINT('Ctrl Pts',(-4.05596218814318,42.5672500034685,-2.35494697412514));
#26826=CARTESIAN_POINT('Ctrl Pts',(-5.30932343282159,42.4402500034686,-4.08005073111972));
#26827=CARTESIAN_POINT('Ctrl Pts',(-6.56268467749997,42.3132500034686,-5.80515448811441));
#26828=CARTESIAN_POINT('Ctrl Pts',(-6.56268467749993,42.1862500034687,-7.93750000000004));
#26829=CARTESIAN_POINT('Ctrl Pts',(-6.56268467750003,42.0592500034685,-10.0698455118856));
#26830=CARTESIAN_POINT('Ctrl Pts',(-5.30932343282159,41.9322500034685,-11.7949492688803));
#26831=CARTESIAN_POINT('Ctrl Pts',(-4.05596218814306,41.8052500034685,-13.5200530258749));
#26832=CARTESIAN_POINT('Ctrl Pts',(-2.02798109407148,41.6782500034687,-14.1789840269267));
#26833=CARTESIAN_POINT('Ctrl Pts',(1.1673575708729E-13,41.5512500034686,
-14.8379150279786));
#26834=CARTESIAN_POINT('Ctrl Pts',(2.02798109407154,41.4242500034688,-14.1789840269267));
#26835=CARTESIAN_POINT('Ctrl Pts',(4.05596218814324,41.2972500034684,-13.5200530258749));
#26836=CARTESIAN_POINT('Ctrl Pts',(5.30932343282159,41.1702500034686,-11.7949492688803));
#26837=CARTESIAN_POINT('Ctrl Pts',(6.56268467750003,41.0432500034686,-10.0698455118856));
#26838=CARTESIAN_POINT('Ctrl Pts',(6.56268467749999,40.9162500034685,-7.93750000000004));
#26839=CARTESIAN_POINT('Ctrl Pts',(6.56268467750014,40.7892500034686,-5.80515448811441));
#26840=CARTESIAN_POINT('Ctrl Pts',(5.30932343282164,40.6622500034686,-4.08005073111972));
#26841=CARTESIAN_POINT('Ctrl Pts',(4.05596218814318,40.5352500034686,-2.35494697412514));
#26842=CARTESIAN_POINT('Ctrl Pts',(2.0279810940716,40.4082500034686,-1.69601597307323));
#26843=CARTESIAN_POINT('Ctrl Pts',(0.,40.2812500034686,-1.0370849720215));
#26844=CARTESIAN_POINT('Ctrl Pts',(-2.02798109407148,40.1542500034686,-1.69601597307323));
#26845=CARTESIAN_POINT('Ctrl Pts',(-4.05596218814312,40.0272500034685,-2.35494697412514));
#26846=CARTESIAN_POINT('Ctrl Pts',(-5.30932343282159,39.9002500034686,-4.08005073111972));
#26847=CARTESIAN_POINT('Ctrl Pts',(-6.56268467749997,39.7732500034686,-5.80515448811441));
#26848=CARTESIAN_POINT('Ctrl Pts',(-6.56268467749987,39.6462500034686,-7.93750000000004));
#26849=CARTESIAN_POINT('Ctrl Pts',(-6.56268467750003,39.5192500034686,-10.0698455118856));
#26850=CARTESIAN_POINT('Ctrl Pts',(-5.30932343282153,39.3922500034687,-11.7949492688803));
#26851=CARTESIAN_POINT('Ctrl Pts',(-4.05596218814318,39.2652500034686,-13.5200530258749));
#26852=CARTESIAN_POINT('Ctrl Pts',(-2.02798109407154,39.1382500034687,-14.1789840269267));
#26853=CARTESIAN_POINT('Ctrl Pts',(0.,39.0112500034685,-14.8379150279786));
#26854=CARTESIAN_POINT('Ctrl Pts',(2.02798109407154,38.8842500034687,-14.1789840269267));
#26855=CARTESIAN_POINT('Ctrl Pts',(4.05596218814312,38.7572500034686,-13.5200530258749));
#26856=CARTESIAN_POINT('Ctrl Pts',(5.30932343282164,38.6302500034687,-11.7949492688803));
#26857=CARTESIAN_POINT('Ctrl Pts',(6.56268467749991,38.5032500034686,-10.0698455118856));
#26858=CARTESIAN_POINT('Ctrl Pts',(6.56268467749999,38.3762500034686,-7.93750000000004));
#26859=CARTESIAN_POINT('Ctrl Pts',(6.56268467750003,38.2492500034685,-5.80515448811441));
#26860=CARTESIAN_POINT('Ctrl Pts',(5.3093234328217,38.1222500034686,-4.08005073111972));
#26861=CARTESIAN_POINT('Ctrl Pts',(4.05596218814312,37.9952500034685,-2.35494697412514));
#26862=CARTESIAN_POINT('Ctrl Pts',(2.0279810940716,37.8682500034686,-1.69601597307323));
#26863=CARTESIAN_POINT('Ctrl Pts',(0.,37.7412500034685,-1.0370849720215));
#26864=CARTESIAN_POINT('Ctrl Pts',(-2.02798109407148,37.6142500034686,-1.69601597307323));
#26865=CARTESIAN_POINT('Ctrl Pts',(-4.05596218814312,37.4872500034686,-2.35494697412514));
#26866=CARTESIAN_POINT('Ctrl Pts',(-5.30932343282153,37.3602500034685,-4.08005073111972));
#26867=CARTESIAN_POINT('Ctrl Pts',(-6.56268467749997,37.2332500034686,-5.80515448811441));
#26868=CARTESIAN_POINT('Ctrl Pts',(-6.56268467749999,37.1062500034686,-7.93750000000004));
#26869=CARTESIAN_POINT('Ctrl Pts',(-6.56268467749997,36.9792500034686,-10.0698455118856));
#26870=CARTESIAN_POINT('Ctrl Pts',(-5.30932343282153,36.8522500034686,-11.7949492688803));
#26871=CARTESIAN_POINT('Ctrl Pts',(-4.05596218814306,36.7252500034685,-13.5200530258749));
#26872=CARTESIAN_POINT('Ctrl Pts',(-2.02798109407154,36.5982500034687,-14.1789840269267));
#26873=CARTESIAN_POINT('Ctrl Pts',(1.1673575708729E-13,36.4712500034686,
-14.8379150279786));
#26874=CARTESIAN_POINT('Ctrl Pts',(2.02798109407154,36.3442500034687,-14.1789840269267));
#26875=CARTESIAN_POINT('Ctrl Pts',(4.05596218814324,36.2172500034686,-13.5200530258749));
#26876=CARTESIAN_POINT('Ctrl Pts',(5.30932343282164,36.0902500034686,-11.7949492688803));
#26877=CARTESIAN_POINT('Ctrl Pts',(6.56268467750008,35.9632500034686,-10.0698455118856));
#26878=CARTESIAN_POINT('Ctrl Pts',(6.56268467749999,35.8362500034687,-7.93750000000004));
#26879=CARTESIAN_POINT('Ctrl Pts',(6.56268467750003,35.7092500034686,-5.80515448811441));
#26880=CARTESIAN_POINT('Ctrl Pts',(5.30932343282159,35.5822500034686,-4.08005073111972));
#26881=CARTESIAN_POINT('Ctrl Pts',(4.05596218814312,35.4552500034686,-2.35494697412514));
#26882=CARTESIAN_POINT('Ctrl Pts',(2.0279810940716,35.3282500034686,-1.69601597307323));
#26883=CARTESIAN_POINT('Ctrl Pts',(5.83678785436452E-14,35.2012500034686,
-1.0370849720215));
#26884=CARTESIAN_POINT('Ctrl Pts',(-2.02798109407148,35.0742500034686,-1.69601597307323));
#26885=CARTESIAN_POINT('Ctrl Pts',(-4.05596218814312,34.9472500034686,-2.35494697412514));
#26886=CARTESIAN_POINT('Ctrl Pts',(-5.30932343282153,34.8202500034686,-4.08005073111972));
#26887=CARTESIAN_POINT('Ctrl Pts',(-6.56268467750003,34.6932500034686,-5.80515448811441));
#26888=CARTESIAN_POINT('Ctrl Pts',(-6.56268467749999,34.5662500034686,-7.93750000000004));
#26889=CARTESIAN_POINT('Ctrl Pts',(-6.56268467749997,34.4392500034686,-10.0698455118856));
#26890=CARTESIAN_POINT('Ctrl Pts',(-5.30932343282148,34.3122500034686,-11.7949492688803));
#26891=CARTESIAN_POINT('Ctrl Pts',(-4.05596218814312,34.1852500034684,-13.5200530258749));
#26892=CARTESIAN_POINT('Ctrl Pts',(-2.02798109407154,34.0582500034686,-14.1789840269267));
#26893=CARTESIAN_POINT('Ctrl Pts',(0.,33.9312500034685,-14.8379150279786));
#26894=CARTESIAN_POINT('Ctrl Pts',(2.0279810940716,33.8042500034687,-14.1789840269267));
#26895=CARTESIAN_POINT('Ctrl Pts',(4.05596218814312,33.6772500034686,-13.5200530258749));
#26896=CARTESIAN_POINT('Ctrl Pts',(5.30932343282164,33.5502500034686,-11.7949492688803));
#26897=CARTESIAN_POINT('Ctrl Pts',(6.56268467750008,33.4232500034685,-10.0698455118856));
#26898=CARTESIAN_POINT('Ctrl Pts',(6.56268467750004,33.2962500034686,-7.93750000000004));
#26899=CARTESIAN_POINT('Ctrl Pts',(6.56268467749991,33.1692500034685,-5.80515448811441));
#26900=CARTESIAN_POINT('Ctrl Pts',(5.30932343282159,33.0422500034686,-4.08005073111972));
#26901=CARTESIAN_POINT('Ctrl Pts',(4.05596218814324,32.9152500034685,-2.35494697412514));
#26902=CARTESIAN_POINT('Ctrl Pts',(2.02798109407165,32.7882500034686,-1.69601597307323));
#26903=CARTESIAN_POINT('Ctrl Pts',(0.,32.6612500034685,-1.0370849720215));
#26904=CARTESIAN_POINT('Ctrl Pts',(-2.02798109407154,32.5342500034686,-1.69601597307323));
#26905=CARTESIAN_POINT('Ctrl Pts',(-4.05596218814312,32.4072500034686,-2.35494697412514));
#26906=CARTESIAN_POINT('Ctrl Pts',(-5.30932343282148,32.2802500034686,-4.08005073111972));
#26907=CARTESIAN_POINT('Ctrl Pts',(-6.56268467749991,32.1532500034685,-5.80515448811441));
#26908=CARTESIAN_POINT('Ctrl Pts',(-6.56268467749999,32.0262500034685,-7.93750000000004));
#26909=CARTESIAN_POINT('Ctrl Pts',(-6.56268467749997,31.8992500034685,-10.0698455118856));
#26910=CARTESIAN_POINT('Ctrl Pts',(-5.30932343282159,31.7722500034686,-11.7949492688803));
#26911=CARTESIAN_POINT('Ctrl Pts',(-4.05596218814312,31.6452500034686,-13.5200530258749));
#26912=CARTESIAN_POINT('Ctrl Pts',(-2.02798109407148,31.5182500034687,-14.1789840269267));
#26913=CARTESIAN_POINT('Ctrl Pts',(0.,31.3912500034685,-14.8379150279786));
#26914=CARTESIAN_POINT('Ctrl Pts',(2.0279810940716,31.2642500034687,-14.1789840269267));
#26915=CARTESIAN_POINT('Ctrl Pts',(4.05596218814312,31.1372500034686,-13.5200530258749));
#26916=CARTESIAN_POINT('Ctrl Pts',(5.30932343282159,31.0102500034686,-11.7949492688803));
#26917=CARTESIAN_POINT('Ctrl Pts',(6.56268467749997,30.8832500034686,-10.0698455118856));
#26918=CARTESIAN_POINT('Ctrl Pts',(6.56268467750004,30.7562500034686,-7.93750000000004));
#26919=CARTESIAN_POINT('Ctrl Pts',(6.56268467750003,30.6292500034685,-5.80515448811441));
#26920=CARTESIAN_POINT('Ctrl Pts',(5.30932343282159,30.5022500034686,-4.08005073111972));
#26921=CARTESIAN_POINT('Ctrl Pts',(4.05596218814312,30.3752500034686,-2.35494697412514));
#26922=CARTESIAN_POINT('Ctrl Pts',(2.02798109407154,30.2482500034685,-1.69601597307323));
#26923=CARTESIAN_POINT('Ctrl Pts',(0.,30.1212500034685,-1.0370849720215));
#26924=CARTESIAN_POINT('Ctrl Pts',(-2.02798109407154,29.9942500034686,-1.69601597307323));
#26925=CARTESIAN_POINT('Ctrl Pts',(-4.05596218814312,29.8672500034686,-2.35494697412503));
#26926=CARTESIAN_POINT('Ctrl Pts',(-5.30932343282148,29.7402500034687,-4.08005073111972));
#26927=CARTESIAN_POINT('Ctrl Pts',(-6.56268467750003,29.6132500034685,-5.80515448811441));
#26928=CARTESIAN_POINT('Ctrl Pts',(-6.56268467749993,29.4862500034685,-7.93750000000004));
#26929=CARTESIAN_POINT('Ctrl Pts',(-6.56268467749997,29.3592500034685,-10.0698455118856));
#26930=CARTESIAN_POINT('Ctrl Pts',(-5.30932343282159,29.2322500034685,-11.7949492688803));
#26931=CARTESIAN_POINT('Ctrl Pts',(-4.05596218814312,29.1052500034686,-13.5200530258749));
#26932=CARTESIAN_POINT('Ctrl Pts',(-2.02798109407148,28.9782500034687,-14.1789840269267));
#26933=CARTESIAN_POINT('Ctrl Pts',(0.,28.8512500034685,-14.8379150279786));
#26934=CARTESIAN_POINT('Ctrl Pts',(2.0279810940716,28.7242500034687,-14.1789840269267));
#26935=CARTESIAN_POINT('Ctrl Pts',(4.05596218814318,28.5972500034685,-13.5200530258749));
#26936=CARTESIAN_POINT('Ctrl Pts',(5.30932343282159,28.4702500034686,-11.7949492688803));
#26937=CARTESIAN_POINT('Ctrl Pts',(6.56268467750008,28.3432500034685,-10.0698455118856));
#26938=CARTESIAN_POINT('Ctrl Pts',(6.56268467749999,28.2162500034686,-7.93750000000004));
#26939=CARTESIAN_POINT('Ctrl Pts',(6.56268467749997,28.0892500034686,-5.80515448811441));
#26940=CARTESIAN_POINT('Ctrl Pts',(5.30932343282164,27.9622500034686,-4.08005073111972));
#26941=CARTESIAN_POINT('Ctrl Pts',(4.05596218814312,27.8352500034686,-2.35494697412514));
#26942=CARTESIAN_POINT('Ctrl Pts',(2.02798109407154,27.7082500034687,-1.69601597307323));
#26943=CARTESIAN_POINT('Ctrl Pts',(0.,27.5812500034685,-1.0370849720215));
#26944=CARTESIAN_POINT('Ctrl Pts',(-2.02798109407148,27.4542500034686,-1.69601597307323));
#26945=CARTESIAN_POINT('Ctrl Pts',(-4.05596218814312,27.3272500034686,-2.35494697412503));
#26946=CARTESIAN_POINT('Ctrl Pts',(-5.30932343282159,27.2002500034686,-4.08005073111972));
#26947=CARTESIAN_POINT('Ctrl Pts',(-6.56268467750003,27.0732500034685,-5.80515448811441));
#26948=CARTESIAN_POINT('Ctrl Pts',(-6.56268467749993,26.9462500034687,-7.93750000000004));
#26949=CARTESIAN_POINT('Ctrl Pts',(-6.56268467749991,26.8192500034686,-10.0698455118856));
#26950=CARTESIAN_POINT('Ctrl Pts',(-5.30932343282159,26.6922500034685,-11.7949492688803));
#26951=CARTESIAN_POINT('Ctrl Pts',(-4.05596218814312,26.5652500034685,-13.5200530258749));
#26952=CARTESIAN_POINT('Ctrl Pts',(-2.02798109407148,26.4382500034687,-14.1789840269267));
#26953=CARTESIAN_POINT('Ctrl Pts',(0.,26.3112500034686,-14.8379150279786));
#26954=CARTESIAN_POINT('Ctrl Pts',(2.02798109407165,26.1842500034687,-14.1789840269267));
#26955=CARTESIAN_POINT('Ctrl Pts',(4.05596218814318,26.0572500034686,-13.5200530258749));
#26956=CARTESIAN_POINT('Ctrl Pts',(5.30932343282159,25.9302500034686,-11.7949492688803));
#26957=CARTESIAN_POINT('Ctrl Pts',(6.56268467750003,25.8032500034686,-10.0698455118856));
#26958=CARTESIAN_POINT('Ctrl Pts',(6.56268467749999,25.6762500034685,-7.93750000000004));
#26959=CARTESIAN_POINT('Ctrl Pts',(6.56268467749997,25.5492500034686,-5.80515448811441));
#26960=CARTESIAN_POINT('Ctrl Pts',(5.30932343282164,25.4222500034686,-4.08005073111972));
#26961=CARTESIAN_POINT('Ctrl Pts',(4.05596218814312,25.2952500034686,-2.35494697412514));
#26962=CARTESIAN_POINT('Ctrl Pts',(2.0279810940716,25.1682500034687,-1.69601597307323));
#26963=CARTESIAN_POINT('Ctrl Pts',(0.,25.0412500034686,-1.0370849720215));
#26964=CARTESIAN_POINT('Ctrl Pts',(-2.02798109407148,24.9142500034685,-1.69601597307323));
#26965=CARTESIAN_POINT('Ctrl Pts',(-4.05596218814318,24.7872500034685,-2.35494697412503));
#26966=CARTESIAN_POINT('Ctrl Pts',(-5.30932343282159,24.6602500034686,-4.08005073111972));
#26967=CARTESIAN_POINT('Ctrl Pts',(-6.56268467750003,24.5332500034686,-5.80515448811441));
#26968=CARTESIAN_POINT('Ctrl Pts',(-6.56268467749987,24.4062500034686,-7.93750000000004));
#26969=CARTESIAN_POINT('Ctrl Pts',(-6.56268467750003,24.2792500034686,-10.0698455118856));
#26970=CARTESIAN_POINT('Ctrl Pts',(-5.30932343282153,24.1522500034687,-11.7949492688803));
#26971=CARTESIAN_POINT('Ctrl Pts',(-4.05596218814324,24.0252500034686,-13.5200530258749));
#26972=CARTESIAN_POINT('Ctrl Pts',(-2.02798109407154,23.8982500034687,-14.1789840269267));
#26973=CARTESIAN_POINT('Ctrl Pts',(0.,23.7712500034685,-14.8379150279786));
#26974=CARTESIAN_POINT('Ctrl Pts',(2.02798109407154,23.6442500034687,-14.1789840269267));
#26975=CARTESIAN_POINT('Ctrl Pts',(4.05596218814318,23.5172500034685,-13.5200530258749));
#26976=CARTESIAN_POINT('Ctrl Pts',(5.30932343282164,23.3902500034686,-11.7949492688803));
#26977=CARTESIAN_POINT('Ctrl Pts',(6.56268467750003,23.2632500034686,-10.0698455118856));
#26978=CARTESIAN_POINT('Ctrl Pts',(6.56268467749999,23.1362500034686,-7.93750000000004));
#26979=CARTESIAN_POINT('Ctrl Pts',(6.56268467750008,23.0092500034686,-5.80515448811441));
#26980=CARTESIAN_POINT('Ctrl Pts',(5.3093234328217,22.8822500034686,-4.08005073111972));
#26981=CARTESIAN_POINT('Ctrl Pts',(4.05596218814318,22.7552500034685,-2.35494697412503));
#26982=CARTESIAN_POINT('Ctrl Pts',(2.0279810940716,22.6282500034686,-1.69601597307323));
#26983=CARTESIAN_POINT('Ctrl Pts',(-1.1673575708729E-13,22.5012500034685,
-1.0370849720215));
#26984=CARTESIAN_POINT('Ctrl Pts',(-2.02798109407148,22.3742500034686,-1.69601597307323));
#26985=CARTESIAN_POINT('Ctrl Pts',(-4.05596218814306,22.2472500034686,-2.35494697412503));
#26986=CARTESIAN_POINT('Ctrl Pts',(-5.30932343282153,22.1202500034686,-4.08005073111972));
#26987=CARTESIAN_POINT('Ctrl Pts',(-6.56268467749997,21.9932500034685,-5.80515448811441));
#26988=CARTESIAN_POINT('Ctrl Pts',(-6.56268467749987,21.8662500034686,-7.93750000000004));
#26989=CARTESIAN_POINT('Ctrl Pts',(-6.56268467750003,21.7392500034685,-10.0698455118856));
#26990=CARTESIAN_POINT('Ctrl Pts',(-5.30932343282153,21.6122500034686,-11.7949492688803));
#26991=CARTESIAN_POINT('Ctrl Pts',(-4.05596218814318,21.4852500034685,-13.5200530258749));
#26992=CARTESIAN_POINT('Ctrl Pts',(-2.02798109407154,21.3582500034687,-14.1789840269267));
#26993=CARTESIAN_POINT('Ctrl Pts',(0.,21.2312500034686,-14.8379150279786));
#26994=CARTESIAN_POINT('Ctrl Pts',(2.02798109407154,21.1042500034687,-14.1789840269267));
#26995=CARTESIAN_POINT('Ctrl Pts',(4.05596218814312,20.9772500034686,-13.5200530258749));
#26996=CARTESIAN_POINT('Ctrl Pts',(5.30932343282164,20.8502500034686,-11.7949492688803));
#26997=CARTESIAN_POINT('Ctrl Pts',(6.56268467749991,20.7232500034686,-10.0698455118856));
#26998=CARTESIAN_POINT('Ctrl Pts',(6.56268467749999,20.5962500034686,-7.93750000000004));
#26999=CARTESIAN_POINT('Ctrl Pts',(6.56268467749997,20.4692500034686,-5.80515448811441));
#27000=CARTESIAN_POINT('Ctrl Pts',(5.3093234328217,20.3422500034686,-4.08005073111972));
#27001=CARTESIAN_POINT('Ctrl Pts',(4.65426917438044,20.2758749729855,-3.17844589287373));
#27002=CARTESIAN_POINT('Ctrl Pts',(3.73830600779964,20.2061014294359,-2.54362399397772));
#27003=CARTESIAN_POINT('Ctrl Pts',(0.0390188495637537,19.9243080309083,
0.0202220033661115));
#27004=CARTESIAN_POINT('Ctrl Pts',(-3.66026830867225,19.6425146323806,2.58406800071006));
#27005=CARTESIAN_POINT('Ctrl Pts',(-7.93751285522927,76.0000074219705,-7.93749999999999));
#27006=CARTESIAN_POINT('Ctrl Pts',(-7.93751285522931,75.8730074219702,-10.5165542657659));
#27007=CARTESIAN_POINT('Ctrl Pts',(-6.42158279295009,75.7460074219701,-12.6030529961856));
#27008=CARTESIAN_POINT('Ctrl Pts',(-4.905652730671,75.6190074219701,-14.6895517266055));
#27009=CARTESIAN_POINT('Ctrl Pts',(-2.45282636533548,75.4920074219701,-15.4865233241424));
#27010=CARTESIAN_POINT('Ctrl Pts',(5.83684243132838E-14,75.36500742197,
-16.2834949216793));
#27011=CARTESIAN_POINT('Ctrl Pts',(2.45282636533542,75.2380074219704,-15.4865233241424));
#27012=CARTESIAN_POINT('Ctrl Pts',(4.905652730671,75.11100742197,-14.6895517266055));
#27013=CARTESIAN_POINT('Ctrl Pts',(6.42158279295009,74.9840074219701,-12.6030529961856));
#27014=CARTESIAN_POINT('Ctrl Pts',(7.93751285522931,74.8570074219701,-10.5165542657659));
#27015=CARTESIAN_POINT('Ctrl Pts',(7.93751285522933,74.7300074219701,-7.93749999999999));
#27016=CARTESIAN_POINT('Ctrl Pts',(7.93751285522926,74.6030074219699,-5.35844573423412));
#27017=CARTESIAN_POINT('Ctrl Pts',(6.42158279295014,74.4760074219701,-3.27194700381432));
#27018=CARTESIAN_POINT('Ctrl Pts',(4.90565273067095,74.3490074219701,-1.18544827339454));
#27019=CARTESIAN_POINT('Ctrl Pts',(2.45282636533548,74.2220074219701,-0.388476675857597));
#27020=CARTESIAN_POINT('Ctrl Pts',(1.16736848626568E-13,74.09500742197,
0.408494921679244));
#27021=CARTESIAN_POINT('Ctrl Pts',(-2.45282636533548,73.9680074219701,-0.388476675857597));
#27022=CARTESIAN_POINT('Ctrl Pts',(-4.90565273067095,73.8410074219701,-1.18544827339454));
#27023=CARTESIAN_POINT('Ctrl Pts',(-6.42158279295014,73.7140074219701,-3.27194700381421));
#27024=CARTESIAN_POINT('Ctrl Pts',(-7.93751285522926,73.58700742197,-5.35844573423412));
#27025=CARTESIAN_POINT('Ctrl Pts',(-7.93751285522933,73.4600074219702,-7.93749999999999));
#27026=CARTESIAN_POINT('Ctrl Pts',(-7.93751285522931,73.33300742197,-10.5165542657659));
#27027=CARTESIAN_POINT('Ctrl Pts',(-6.42158279295009,73.2060074219702,-12.6030529961856));
#27028=CARTESIAN_POINT('Ctrl Pts',(-4.90565273067083,73.07900742197,-14.6895517266055));
#27029=CARTESIAN_POINT('Ctrl Pts',(-2.45282636533553,72.9520074219703,-15.4865233241424));
#27030=CARTESIAN_POINT('Ctrl Pts',(5.83684243132838E-14,72.82500742197,
-16.2834949216793));
#27031=CARTESIAN_POINT('Ctrl Pts',(2.45282636533548,72.6980074219702,-15.4865233241424));
#27032=CARTESIAN_POINT('Ctrl Pts',(4.90565273067089,72.5710074219701,-14.6895517266055));
#27033=CARTESIAN_POINT('Ctrl Pts',(6.42158279295014,72.4440074219703,-12.6030529961856));
#27034=CARTESIAN_POINT('Ctrl Pts',(7.93751285522931,72.3170074219701,-10.5165542657659));
#27035=CARTESIAN_POINT('Ctrl Pts',(7.93751285522939,72.1900074219701,-7.93749999999999));
#27036=CARTESIAN_POINT('Ctrl Pts',(7.93751285522931,72.0630074219699,-5.35844573423412));
#27037=CARTESIAN_POINT('Ctrl Pts',(6.4215827929502,71.93600742197,-3.27194700381432));
#27038=CARTESIAN_POINT('Ctrl Pts',(4.905652730671,71.80900742197,-1.18544827339454));
#27039=CARTESIAN_POINT('Ctrl Pts',(2.45282636533537,71.6820074219701,-0.388476675857597));
#27040=CARTESIAN_POINT('Ctrl Pts',(0.,71.55500742197,0.408494921679244));
#27041=CARTESIAN_POINT('Ctrl Pts',(-2.45282636533548,71.4280074219701,-0.388476675857597));
#27042=CARTESIAN_POINT('Ctrl Pts',(-4.90565273067095,71.3010074219701,-1.18544827339454));
#27043=CARTESIAN_POINT('Ctrl Pts',(-6.42158279295009,71.1740074219701,-3.27194700381421));
#27044=CARTESIAN_POINT('Ctrl Pts',(-7.93751285522926,71.0470074219702,-5.35844573423412));
#27045=CARTESIAN_POINT('Ctrl Pts',(-7.93751285522927,70.9200074219701,-7.93749999999999));
#27046=CARTESIAN_POINT('Ctrl Pts',(-7.9375128552292,70.7930074219701,-10.5165542657659));
#27047=CARTESIAN_POINT('Ctrl Pts',(-6.42158279295009,70.6660074219703,-12.6030529961856));
#27048=CARTESIAN_POINT('Ctrl Pts',(-4.90565273067095,70.5390074219701,-14.6895517266055));
#27049=CARTESIAN_POINT('Ctrl Pts',(-2.45282636533553,70.4120074219703,-15.4865233241424));
#27050=CARTESIAN_POINT('Ctrl Pts',(5.4576963861738E-19,70.2850074219701,
-16.2834949216793));
#27051=CARTESIAN_POINT('Ctrl Pts',(2.45282636533548,70.1580074219703,-15.4865233241424));
#27052=CARTESIAN_POINT('Ctrl Pts',(4.90565273067089,70.0310074219701,-14.6895517266055));
#27053=CARTESIAN_POINT('Ctrl Pts',(6.42158279295014,69.9040074219702,-12.6030529961856));
#27054=CARTESIAN_POINT('Ctrl Pts',(7.93751285522937,69.77700742197,-10.5165542657659));
#27055=CARTESIAN_POINT('Ctrl Pts',(7.93751285522939,69.6500074219702,-7.93749999999999));
#27056=CARTESIAN_POINT('Ctrl Pts',(7.93751285522931,69.5230074219701,-5.35844573423412));
#27057=CARTESIAN_POINT('Ctrl Pts',(6.4215827929502,69.39600742197,-3.27194700381432));
#27058=CARTESIAN_POINT('Ctrl Pts',(4.90565273067089,69.26900742197,-1.18544827339454));
#27059=CARTESIAN_POINT('Ctrl Pts',(2.45282636533542,69.14200742197,-0.388476675857597));
#27060=CARTESIAN_POINT('Ctrl Pts',(1.09153927723476E-18,69.0150074219701,
0.408494921679244));
#27061=CARTESIAN_POINT('Ctrl Pts',(-2.45282636533542,68.88800742197,-0.388476675857597));
#27062=CARTESIAN_POINT('Ctrl Pts',(-4.90565273067095,68.76100742197,-1.18544827339454));
#27063=CARTESIAN_POINT('Ctrl Pts',(-6.42158279295009,68.6340074219701,-3.27194700381421));
#27064=CARTESIAN_POINT('Ctrl Pts',(-7.93751285522937,68.5070074219701,-5.35844573423412));
#27065=CARTESIAN_POINT('Ctrl Pts',(-7.93751285522927,68.3800074219701,-7.93749999999999));
#27066=CARTESIAN_POINT('Ctrl Pts',(-7.93751285522926,68.25300742197,-10.5165542657659));
#27067=CARTESIAN_POINT('Ctrl Pts',(-6.42158279295009,68.1260074219703,-12.6030529961856));
#27068=CARTESIAN_POINT('Ctrl Pts',(-4.90565273067095,67.9990074219701,-14.6895517266055));
#27069=CARTESIAN_POINT('Ctrl Pts',(-2.45282636533548,67.8720074219703,-15.4865233241424));
#27070=CARTESIAN_POINT('Ctrl Pts',(1.16736848626568E-13,67.74500742197,
-16.2834949216793));
#27071=CARTESIAN_POINT('Ctrl Pts',(2.45282636533548,67.6180074219702,-15.4865233241424));
#27072=CARTESIAN_POINT('Ctrl Pts',(4.90565273067089,67.4910074219701,-14.6895517266055));
#27073=CARTESIAN_POINT('Ctrl Pts',(6.4215827929502,67.3640074219702,-12.6030529961856));
#27074=CARTESIAN_POINT('Ctrl Pts',(7.93751285522926,67.2370074219701,-10.5165542657659));
#27075=CARTESIAN_POINT('Ctrl Pts',(7.93751285522939,67.1100074219701,-7.93749999999999));
#27076=CARTESIAN_POINT('Ctrl Pts',(7.93751285522931,66.9830074219701,-5.35844573423412));
#27077=CARTESIAN_POINT('Ctrl Pts',(6.4215827929502,66.85600742197,-3.27194700381432));
#27078=CARTESIAN_POINT('Ctrl Pts',(4.905652730671,66.72900742197,-1.18544827339454));
#27079=CARTESIAN_POINT('Ctrl Pts',(2.45282636533542,66.6020074219701,-0.388476675857597));
#27080=CARTESIAN_POINT('Ctrl Pts',(-5.4576963861738E-19,66.4750074219701,
0.408494921679244));
#27081=CARTESIAN_POINT('Ctrl Pts',(-2.45282636533553,66.3480074219701,-0.388476675857597));
#27082=CARTESIAN_POINT('Ctrl Pts',(-4.90565273067089,66.2210074219701,-1.18544827339454));
#27083=CARTESIAN_POINT('Ctrl Pts',(-6.42158279295009,66.09400742197,-3.27194700381421));
#27084=CARTESIAN_POINT('Ctrl Pts',(-7.9375128552292,65.96700742197,-5.35844573423412));
#27085=CARTESIAN_POINT('Ctrl Pts',(-7.93751285522927,65.8400074219701,-7.93749999999999));
#27086=CARTESIAN_POINT('Ctrl Pts',(-7.93751285522926,65.7130074219699,-10.5165542657659));
#27087=CARTESIAN_POINT('Ctrl Pts',(-6.42158279295003,65.5860074219702,-12.6030529961856));
#27088=CARTESIAN_POINT('Ctrl Pts',(-4.90565273067095,65.45900742197,-14.6895517266055));
#27089=CARTESIAN_POINT('Ctrl Pts',(-2.45282636533548,65.3320074219702,-15.4865233241424));
#27090=CARTESIAN_POINT('Ctrl Pts',(-1.09153927723476E-18,65.20500742197,
-16.2834949216793));
#27091=CARTESIAN_POINT('Ctrl Pts',(2.45282636533537,65.0780074219702,-15.4865233241424));
#27092=CARTESIAN_POINT('Ctrl Pts',(4.90565273067095,64.9510074219701,-14.6895517266055));
#27093=CARTESIAN_POINT('Ctrl Pts',(6.4215827929502,64.8240074219702,-12.6030529961856));
#27094=CARTESIAN_POINT('Ctrl Pts',(7.93751285522937,64.6970074219701,-10.5165542657659));
#27095=CARTESIAN_POINT('Ctrl Pts',(7.93751285522927,64.5700074219701,-7.93749999999999));
#27096=CARTESIAN_POINT('Ctrl Pts',(7.93751285522931,64.4430074219701,-5.35844573423412));
#27097=CARTESIAN_POINT('Ctrl Pts',(6.42158279295009,64.3160074219702,-3.27194700381421));
#27098=CARTESIAN_POINT('Ctrl Pts',(4.90565273067089,64.1890074219699,-1.18544827339454));
#27099=CARTESIAN_POINT('Ctrl Pts',(2.45282636533548,64.0620074219701,-0.388476675857597));
#27100=CARTESIAN_POINT('Ctrl Pts',(0.,63.9350074219701,0.408494921679244));
#27101=CARTESIAN_POINT('Ctrl Pts',(-2.45282636533548,63.8080074219701,-0.388476675857597));
#27102=CARTESIAN_POINT('Ctrl Pts',(-4.90565273067089,63.68100742197,-1.18544827339454));
#27103=CARTESIAN_POINT('Ctrl Pts',(-6.42158279295009,63.5540074219701,-3.27194700381421));
#27104=CARTESIAN_POINT('Ctrl Pts',(-7.93751285522931,63.4270074219701,-5.35844573423412));
#27105=CARTESIAN_POINT('Ctrl Pts',(-7.93751285522927,63.3000074219701,-7.93749999999999));
#27106=CARTESIAN_POINT('Ctrl Pts',(-7.93751285522926,63.1730074219701,-10.5165542657659));
#27107=CARTESIAN_POINT('Ctrl Pts',(-6.42158279295003,63.0460074219702,-12.6030529961856));
#27108=CARTESIAN_POINT('Ctrl Pts',(-4.90565273067095,62.9190074219701,-14.6895517266055));
#27109=CARTESIAN_POINT('Ctrl Pts',(-2.45282636533548,62.7920074219702,-15.4865233241424));
#27110=CARTESIAN_POINT('Ctrl Pts',(0.,62.66500742197,-16.2834949216793));
#27111=CARTESIAN_POINT('Ctrl Pts',(2.45282636533542,62.5380074219702,-15.4865233241424));
#27112=CARTESIAN_POINT('Ctrl Pts',(4.90565273067095,62.41100742197,-14.6895517266055));
#27113=CARTESIAN_POINT('Ctrl Pts',(6.42158279295009,62.2840074219701,-12.6030529961856));
#27114=CARTESIAN_POINT('Ctrl Pts',(7.93751285522926,62.1570074219701,-10.5165542657659));
#27115=CARTESIAN_POINT('Ctrl Pts',(7.93751285522933,62.0300074219701,-7.93749999999999));
#27116=CARTESIAN_POINT('Ctrl Pts',(7.93751285522937,61.9030074219701,-5.35844573423412));
#27117=CARTESIAN_POINT('Ctrl Pts',(6.42158279295009,61.7760074219701,-3.27194700381421));
#27118=CARTESIAN_POINT('Ctrl Pts',(4.90565273067095,61.6490074219701,-1.18544827339454));
#27119=CARTESIAN_POINT('Ctrl Pts',(2.45282636533548,61.5220074219701,-0.388476675857597));
#27120=CARTESIAN_POINT('Ctrl Pts',(0.,61.3950074219701,0.408494921679244));
#27121=CARTESIAN_POINT('Ctrl Pts',(-2.45282636533548,61.2680074219701,-0.388476675857598));
#27122=CARTESIAN_POINT('Ctrl Pts',(-4.905652730671,61.1410074219701,-1.18544827339454));
#27123=CARTESIAN_POINT('Ctrl Pts',(-6.42158279295003,61.0140074219702,-3.27194700381421));
#27124=CARTESIAN_POINT('Ctrl Pts',(-7.93751285522931,60.88700742197,-5.35844573423412));
#27125=CARTESIAN_POINT('Ctrl Pts',(-7.93751285522922,60.76000742197,-7.93749999999999));
#27126=CARTESIAN_POINT('Ctrl Pts',(-7.93751285522926,60.63300742197,-10.5165542657659));
#27127=CARTESIAN_POINT('Ctrl Pts',(-6.42158279295009,60.5060074219702,-12.6030529961856));
#27128=CARTESIAN_POINT('Ctrl Pts',(-4.90565273067089,60.3790074219701,-14.6895517266055));
#27129=CARTESIAN_POINT('Ctrl Pts',(-2.45282636533548,60.2520074219701,-15.4865233241424));
#27130=CARTESIAN_POINT('Ctrl Pts',(-1.09153927723476E-18,60.12500742197,
-16.2834949216793));
#27131=CARTESIAN_POINT('Ctrl Pts',(2.45282636533542,59.9980074219701,-15.4865233241424));
#27132=CARTESIAN_POINT('Ctrl Pts',(4.90565273067095,59.8710074219699,-14.6895517266055));
#27133=CARTESIAN_POINT('Ctrl Pts',(6.42158279295009,59.7440074219701,-12.6030529961856));
#27134=CARTESIAN_POINT('Ctrl Pts',(7.93751285522931,59.6170074219701,-10.5165542657659));
#27135=CARTESIAN_POINT('Ctrl Pts',(7.93751285522933,59.4900074219701,-7.93749999999999));
#27136=CARTESIAN_POINT('Ctrl Pts',(7.93751285522937,59.36300742197,-5.35844573423412));
#27137=CARTESIAN_POINT('Ctrl Pts',(6.42158279295014,59.2360074219701,-3.27194700381421));
#27138=CARTESIAN_POINT('Ctrl Pts',(4.90565273067095,59.1090074219701,-1.18544827339454));
#27139=CARTESIAN_POINT('Ctrl Pts',(2.45282636533548,58.9820074219701,-0.388476675857597));
#27140=CARTESIAN_POINT('Ctrl Pts',(-5.4576963861738E-19,58.85500742197,
0.408494921679244));
#27141=CARTESIAN_POINT('Ctrl Pts',(-2.45282636533548,58.7280074219701,-0.388476675857598));
#27142=CARTESIAN_POINT('Ctrl Pts',(-4.90565273067089,58.6010074219702,-1.18544827339454));
#27143=CARTESIAN_POINT('Ctrl Pts',(-6.42158279295009,58.4740074219701,-3.27194700381421));
#27144=CARTESIAN_POINT('Ctrl Pts',(-7.9375128552292,58.3470074219701,-5.35844573423412));
#27145=CARTESIAN_POINT('Ctrl Pts',(-7.93751285522922,58.2200074219702,-7.93749999999999));
#27146=CARTESIAN_POINT('Ctrl Pts',(-7.93751285522931,58.0930074219701,-10.5165542657659));
#27147=CARTESIAN_POINT('Ctrl Pts',(-6.42158279295009,57.9660074219701,-12.6030529961856));
#27148=CARTESIAN_POINT('Ctrl Pts',(-4.90565273067089,57.83900742197,-14.6895517266055));
#27149=CARTESIAN_POINT('Ctrl Pts',(-2.45282636533542,57.7120074219702,-15.4865233241424));
#27150=CARTESIAN_POINT('Ctrl Pts',(0.,57.5850074219701,-16.2834949216793));
#27151=CARTESIAN_POINT('Ctrl Pts',(2.45282636533548,57.4580074219702,-15.4865233241424));
#27152=CARTESIAN_POINT('Ctrl Pts',(4.90565273067095,57.33100742197,-14.6895517266055));
#27153=CARTESIAN_POINT('Ctrl Pts',(6.42158279295014,57.2040074219703,-12.6030529961856));
#27154=CARTESIAN_POINT('Ctrl Pts',(7.93751285522931,57.07700742197,-10.5165542657659));
#27155=CARTESIAN_POINT('Ctrl Pts',(7.93751285522939,56.95000742197,-7.93749999999999));
#27156=CARTESIAN_POINT('Ctrl Pts',(7.93751285522926,56.8230074219701,-5.35844573423412));
#27157=CARTESIAN_POINT('Ctrl Pts',(6.42158279295014,56.6960074219701,-3.27194700381421));
#27158=CARTESIAN_POINT('Ctrl Pts',(4.90565273067095,56.5690074219701,-1.18544827339454));
#27159=CARTESIAN_POINT('Ctrl Pts',(2.45282636533548,56.4420074219701,-0.388476675857598));
#27160=CARTESIAN_POINT('Ctrl Pts',(0.,56.3150074219701,0.408494921679244));
#27161=CARTESIAN_POINT('Ctrl Pts',(-2.45282636533548,56.1880074219701,-0.388476675857598));
#27162=CARTESIAN_POINT('Ctrl Pts',(-4.90565273067095,56.06100742197,-1.18544827339454));
#27163=CARTESIAN_POINT('Ctrl Pts',(-6.42158279295009,55.9340074219701,-3.27194700381421));
#27164=CARTESIAN_POINT('Ctrl Pts',(-7.93751285522931,55.80700742197,-5.35844573423412));
#27165=CARTESIAN_POINT('Ctrl Pts',(-7.93751285522927,55.6800074219702,-7.93749999999999));
#27166=CARTESIAN_POINT('Ctrl Pts',(-7.9375128552292,55.5530074219702,-10.5165542657659));
#27167=CARTESIAN_POINT('Ctrl Pts',(-6.42158279295009,55.4260074219702,-12.6030529961856));
#27168=CARTESIAN_POINT('Ctrl Pts',(-4.90565273067089,55.2990074219701,-14.6895517266055));
#27169=CARTESIAN_POINT('Ctrl Pts',(-2.45282636533548,55.1720074219703,-15.4865233241424));
#27170=CARTESIAN_POINT('Ctrl Pts',(-1.16736848626568E-13,55.04500742197,
-16.2834949216793));
#27171=CARTESIAN_POINT('Ctrl Pts',(2.45282636533548,54.9180074219703,-15.4865233241424));
#27172=CARTESIAN_POINT('Ctrl Pts',(4.90565273067083,54.7910074219699,-14.6895517266055));
#27173=CARTESIAN_POINT('Ctrl Pts',(6.42158279295014,54.6640074219702,-12.6030529961857));
#27174=CARTESIAN_POINT('Ctrl Pts',(7.93751285522931,54.53700742197,-10.5165542657659));
#27175=CARTESIAN_POINT('Ctrl Pts',(7.93751285522939,54.4100074219701,-7.93750000000004));
#27176=CARTESIAN_POINT('Ctrl Pts',(7.93751285522937,54.2830074219701,-5.35844573423412));
#27177=CARTESIAN_POINT('Ctrl Pts',(6.4215827929502,54.1560074219701,-3.27194700381427));
#27178=CARTESIAN_POINT('Ctrl Pts',(4.90565273067083,54.0290074219701,-1.18544827339454));
#27179=CARTESIAN_POINT('Ctrl Pts',(2.45282636533542,53.90200742197,-0.388476675857653));
#27180=CARTESIAN_POINT('Ctrl Pts',(-5.83684243132838E-14,53.77500742197,
0.408494921679244));
#27181=CARTESIAN_POINT('Ctrl Pts',(-2.45282636533542,53.6480074219701,-0.388476675857653));
#27182=CARTESIAN_POINT('Ctrl Pts',(-4.90565273067095,53.5210074219699,-1.18544827339454));
#27183=CARTESIAN_POINT('Ctrl Pts',(-6.42158279295009,53.39400742197,-3.27194700381427));
#27184=CARTESIAN_POINT('Ctrl Pts',(-7.93751285522926,53.26700742197,-5.35844573423412));
#27185=CARTESIAN_POINT('Ctrl Pts',(-7.93751285522927,53.1400074219701,-7.93750000000004));
#27186=CARTESIAN_POINT('Ctrl Pts',(-7.93751285522931,53.0130074219701,-10.5165542657659));
#27187=CARTESIAN_POINT('Ctrl Pts',(-6.42158279295009,52.8860074219702,-12.6030529961857));
#27188=CARTESIAN_POINT('Ctrl Pts',(-4.905652730671,52.7590074219701,-14.6895517266055));
#27189=CARTESIAN_POINT('Ctrl Pts',(-2.45282636533548,52.6320074219702,-15.4865233241424));
#27190=CARTESIAN_POINT('Ctrl Pts',(1.16736848626568E-13,52.5050074219701,
-16.2834949216793));
#27191=CARTESIAN_POINT('Ctrl Pts',(2.45282636533548,52.3780074219702,-15.4865233241424));
#27192=CARTESIAN_POINT('Ctrl Pts',(4.905652730671,52.2510074219701,-14.6895517266055));
#27193=CARTESIAN_POINT('Ctrl Pts',(6.4215827929502,52.1240074219702,-12.6030529961857));
#27194=CARTESIAN_POINT('Ctrl Pts',(7.93751285522931,51.9970074219699,-10.5165542657659));
#27195=CARTESIAN_POINT('Ctrl Pts',(7.93751285522939,51.8700074219702,-7.93750000000004));
#27196=CARTESIAN_POINT('Ctrl Pts',(7.93751285522931,51.7430074219701,-5.35844573423412));
#27197=CARTESIAN_POINT('Ctrl Pts',(6.4215827929502,51.61600742197,-3.27194700381427));
#27198=CARTESIAN_POINT('Ctrl Pts',(4.90565273067095,51.4890074219701,-1.18544827339454));
#27199=CARTESIAN_POINT('Ctrl Pts',(2.45282636533542,51.3620074219701,-0.388476675857653));
#27200=CARTESIAN_POINT('Ctrl Pts',(1.16736848626568E-13,51.2350074219701,
0.408494921679244));
#27201=CARTESIAN_POINT('Ctrl Pts',(-2.45282636533542,51.1080074219701,-0.388476675857653));
#27202=CARTESIAN_POINT('Ctrl Pts',(-4.90565273067095,50.9810074219701,-1.18544827339454));
#27203=CARTESIAN_POINT('Ctrl Pts',(-6.42158279295009,50.85400742197,-3.27194700381427));
#27204=CARTESIAN_POINT('Ctrl Pts',(-7.93751285522926,50.7270074219701,-5.35844573423412));
#27205=CARTESIAN_POINT('Ctrl Pts',(-7.93751285522927,50.6000074219701,-7.93750000000004));
#27206=CARTESIAN_POINT('Ctrl Pts',(-7.93751285522931,50.47300742197,-10.5165542657659));
#27207=CARTESIAN_POINT('Ctrl Pts',(-6.42158279295003,50.3460074219702,-12.6030529961857));
#27208=CARTESIAN_POINT('Ctrl Pts',(-4.90565273067083,50.2190074219701,-14.6895517266055));
#27209=CARTESIAN_POINT('Ctrl Pts',(-2.45282636533548,50.0920074219702,-15.4865233241424));
#27210=CARTESIAN_POINT('Ctrl Pts',(1.16736848626568E-13,49.9650074219701,
-16.2834949216793));
#27211=CARTESIAN_POINT('Ctrl Pts',(2.45282636533548,49.8380074219702,-15.4865233241424));
#27212=CARTESIAN_POINT('Ctrl Pts',(4.90565273067089,49.7110074219701,-14.6895517266055));
#27213=CARTESIAN_POINT('Ctrl Pts',(6.4215827929502,49.5840074219702,-12.6030529961857));
#27214=CARTESIAN_POINT('Ctrl Pts',(7.93751285522931,49.4570074219702,-10.5165542657659));
#27215=CARTESIAN_POINT('Ctrl Pts',(7.93751285522939,49.3300074219701,-7.93750000000004));
#27216=CARTESIAN_POINT('Ctrl Pts',(7.93751285522931,49.2030074219701,-5.35844573423412));
#27217=CARTESIAN_POINT('Ctrl Pts',(6.4215827929502,49.0760074219702,-3.27194700381427));
#27218=CARTESIAN_POINT('Ctrl Pts',(4.905652730671,48.94900742197,-1.18544827339454));
#27219=CARTESIAN_POINT('Ctrl Pts',(2.45282636533548,48.8220074219701,-0.388476675857653));
#27220=CARTESIAN_POINT('Ctrl Pts',(0.,48.6950074219701,0.408494921679244));
#27221=CARTESIAN_POINT('Ctrl Pts',(-2.45282636533548,48.5680074219701,-0.388476675857653));
#27222=CARTESIAN_POINT('Ctrl Pts',(-4.90565273067095,48.44100742197,-1.18544827339454));
#27223=CARTESIAN_POINT('Ctrl Pts',(-6.42158279295009,48.3140074219701,-3.27194700381427));
#27224=CARTESIAN_POINT('Ctrl Pts',(-7.93751285522926,48.1870074219701,-5.35844573423412));
#27225=CARTESIAN_POINT('Ctrl Pts',(-7.93751285522927,48.06000742197,-7.93750000000004));
#27226=CARTESIAN_POINT('Ctrl Pts',(-7.9375128552292,47.9330074219701,-10.5165542657659));
#27227=CARTESIAN_POINT('Ctrl Pts',(-6.42158279295003,47.8060074219702,-12.6030529961857));
#27228=CARTESIAN_POINT('Ctrl Pts',(-4.90565273067095,47.6790074219701,-14.6895517266055));
#27229=CARTESIAN_POINT('Ctrl Pts',(-2.45282636533548,47.5520074219702,-15.4865233241424));
#27230=CARTESIAN_POINT('Ctrl Pts',(1.09153927723476E-18,47.4250074219701,
-16.2834949216793));
#27231=CARTESIAN_POINT('Ctrl Pts',(2.45282636533542,47.2980074219702,-15.4865233241424));
#27232=CARTESIAN_POINT('Ctrl Pts',(4.90565273067089,47.17100742197,-14.6895517266055));
#27233=CARTESIAN_POINT('Ctrl Pts',(6.4215827929502,47.0440074219702,-12.6030529961857));
#27234=CARTESIAN_POINT('Ctrl Pts',(7.93751285522937,46.9170074219701,-10.5165542657659));
#27235=CARTESIAN_POINT('Ctrl Pts',(7.93751285522933,46.7900074219701,-7.93750000000004));
#27236=CARTESIAN_POINT('Ctrl Pts',(7.93751285522931,46.66300742197,-5.35844573423412));
#27237=CARTESIAN_POINT('Ctrl Pts',(6.42158279295009,46.5360074219702,-3.27194700381427));
#27238=CARTESIAN_POINT('Ctrl Pts',(4.90565273067089,46.4090074219701,-1.18544827339454));
#27239=CARTESIAN_POINT('Ctrl Pts',(2.45282636533548,46.2820074219701,-0.388476675857653));
#27240=CARTESIAN_POINT('Ctrl Pts',(1.09153927723476E-18,46.15500742197,
0.408494921679244));
#27241=CARTESIAN_POINT('Ctrl Pts',(-2.45282636533548,46.0280074219701,-0.388476675857653));
#27242=CARTESIAN_POINT('Ctrl Pts',(-4.90565273067095,45.9010074219699,-1.18544827339454));
#27243=CARTESIAN_POINT('Ctrl Pts',(-6.42158279295003,45.7740074219702,-3.27194700381427));
#27244=CARTESIAN_POINT('Ctrl Pts',(-7.93751285522931,45.64700742197,-5.35844573423412));
#27245=CARTESIAN_POINT('Ctrl Pts',(-7.93751285522922,45.52000742197,-7.93750000000004));
#27246=CARTESIAN_POINT('Ctrl Pts',(-7.93751285522926,45.39300742197,-10.5165542657659));
#27247=CARTESIAN_POINT('Ctrl Pts',(-6.42158279294998,45.2660074219702,-12.6030529961857));
#27248=CARTESIAN_POINT('Ctrl Pts',(-4.90565273067095,45.13900742197,-14.6895517266055));
#27249=CARTESIAN_POINT('Ctrl Pts',(-2.45282636533548,45.0120074219701,-15.4865233241424));
#27250=CARTESIAN_POINT('Ctrl Pts',(1.16736848626568E-13,44.88500742197,
-16.2834949216792));
#27251=CARTESIAN_POINT('Ctrl Pts',(2.45282636533542,44.7580074219701,-15.4865233241424));
#27252=CARTESIAN_POINT('Ctrl Pts',(4.90565273067095,44.6310074219701,-14.6895517266055));
#27253=CARTESIAN_POINT('Ctrl Pts',(6.42158279295009,44.5040074219701,-12.6030529961857));
#27254=CARTESIAN_POINT('Ctrl Pts',(7.93751285522926,44.37700742197,-10.5165542657659));
#27255=CARTESIAN_POINT('Ctrl Pts',(7.93751285522933,44.2500074219701,-7.93750000000004));
#27256=CARTESIAN_POINT('Ctrl Pts',(7.93751285522931,44.12300742197,-5.35844573423412));
#27257=CARTESIAN_POINT('Ctrl Pts',(6.42158279295014,43.9960074219701,-3.27194700381427));
#27258=CARTESIAN_POINT('Ctrl Pts',(4.905652730671,43.86900742197,-1.18544827339454));
#27259=CARTESIAN_POINT('Ctrl Pts',(2.45282636533548,43.7420074219702,-0.388476675857653));
#27260=CARTESIAN_POINT('Ctrl Pts',(-1.09153927723476E-18,43.6150074219699,
0.408494921679244));
#27261=CARTESIAN_POINT('Ctrl Pts',(-2.45282636533548,43.4880074219701,-0.388476675857653));
#27262=CARTESIAN_POINT('Ctrl Pts',(-4.90565273067089,43.36100742197,-1.18544827339454));
#27263=CARTESIAN_POINT('Ctrl Pts',(-6.42158279294998,43.2340074219701,-3.27194700381427));
#27264=CARTESIAN_POINT('Ctrl Pts',(-7.9375128552292,43.1070074219701,-5.35844573423412));
#27265=CARTESIAN_POINT('Ctrl Pts',(-7.93751285522922,42.9800074219701,-7.93750000000004));
#27266=CARTESIAN_POINT('Ctrl Pts',(-7.93751285522926,42.85300742197,-10.5165542657659));
#27267=CARTESIAN_POINT('Ctrl Pts',(-6.42158279295009,42.7260074219701,-12.6030529961857));
#27268=CARTESIAN_POINT('Ctrl Pts',(-4.90565273067095,42.5990074219699,-14.6895517266055));
#27269=CARTESIAN_POINT('Ctrl Pts',(-2.45282636533542,42.4720074219702,-15.4865233241424));
#27270=CARTESIAN_POINT('Ctrl Pts',(-1.09153927723476E-18,42.3450074219701,
-16.2834949216792));
#27271=CARTESIAN_POINT('Ctrl Pts',(2.45282636533548,42.2180074219702,-15.4865233241424));
#27272=CARTESIAN_POINT('Ctrl Pts',(4.90565273067095,42.0910074219701,-14.6895517266055));
#27273=CARTESIAN_POINT('Ctrl Pts',(6.42158279295014,41.9640074219702,-12.6030529961857));
#27274=CARTESIAN_POINT('Ctrl Pts',(7.93751285522937,41.8370074219701,-10.5165542657659));
#27275=CARTESIAN_POINT('Ctrl Pts',(7.93751285522939,41.71000742197,-7.93750000000004));
#27276=CARTESIAN_POINT('Ctrl Pts',(7.93751285522931,41.5830074219701,-5.35844573423412));
#27277=CARTESIAN_POINT('Ctrl Pts',(6.4215827929502,41.4560074219701,-3.27194700381427));
#27278=CARTESIAN_POINT('Ctrl Pts',(4.90565273067089,41.3290074219701,-1.18544827339454));
#27279=CARTESIAN_POINT('Ctrl Pts',(2.45282636533548,41.2020074219701,-0.388476675857653));
#27280=CARTESIAN_POINT('Ctrl Pts',(0.,41.07500742197,0.408494921679244));
#27281=CARTESIAN_POINT('Ctrl Pts',(-2.45282636533548,40.9480074219701,-0.388476675857653));
#27282=CARTESIAN_POINT('Ctrl Pts',(-4.90565273067089,40.8210074219701,-1.18544827339454));
#27283=CARTESIAN_POINT('Ctrl Pts',(-6.42158279295009,40.6940074219701,-3.27194700381427));
#27284=CARTESIAN_POINT('Ctrl Pts',(-7.93751285522931,40.56700742197,-5.35844573423412));
#27285=CARTESIAN_POINT('Ctrl Pts',(-7.93751285522922,40.4400074219702,-7.93750000000004));
#27286=CARTESIAN_POINT('Ctrl Pts',(-7.93751285522926,40.3130074219699,-10.5165542657659));
#27287=CARTESIAN_POINT('Ctrl Pts',(-6.42158279295009,40.1860074219702,-12.6030529961857));
#27288=CARTESIAN_POINT('Ctrl Pts',(-4.90565273067095,40.05900742197,-14.6895517266055));
#27289=CARTESIAN_POINT('Ctrl Pts',(-2.45282636533542,39.9320074219703,-15.4865233241424));
#27290=CARTESIAN_POINT('Ctrl Pts',(0.,39.80500742197,-16.2834949216792));
#27291=CARTESIAN_POINT('Ctrl Pts',(2.45282636533548,39.6780074219702,-15.4865233241424));
#27292=CARTESIAN_POINT('Ctrl Pts',(4.90565273067095,39.55100742197,-14.6895517266055));
#27293=CARTESIAN_POINT('Ctrl Pts',(6.42158279295014,39.4240074219703,-12.6030529961857));
#27294=CARTESIAN_POINT('Ctrl Pts',(7.93751285522926,39.29700742197,-10.5165542657659));
#27295=CARTESIAN_POINT('Ctrl Pts',(7.93751285522939,39.1700074219701,-7.93750000000004));
#27296=CARTESIAN_POINT('Ctrl Pts',(7.93751285522926,39.04300742197,-5.35844573423412));
#27297=CARTESIAN_POINT('Ctrl Pts',(6.4215827929502,38.91600742197,-3.27194700381427));
#27298=CARTESIAN_POINT('Ctrl Pts',(4.90565273067095,38.78900742197,-1.18544827339454));
#27299=CARTESIAN_POINT('Ctrl Pts',(2.45282636533542,38.6620074219701,-0.388476675857653));
#27300=CARTESIAN_POINT('Ctrl Pts',(0.,38.53500742197,0.408494921679244));
#27301=CARTESIAN_POINT('Ctrl Pts',(-2.45282636533542,38.40800742197,-0.388476675857653));
#27302=CARTESIAN_POINT('Ctrl Pts',(-4.905652730671,38.2810074219701,-1.18544827339454));
#27303=CARTESIAN_POINT('Ctrl Pts',(-6.42158279295009,38.1540074219701,-3.27194700381427));
#27304=CARTESIAN_POINT('Ctrl Pts',(-7.93751285522931,38.02700742197,-5.35844573423412));
#27305=CARTESIAN_POINT('Ctrl Pts',(-7.93751285522927,37.9000074219701,-7.93750000000004));
#27306=CARTESIAN_POINT('Ctrl Pts',(-7.93751285522926,37.7730074219701,-10.5165542657659));
#27307=CARTESIAN_POINT('Ctrl Pts',(-6.42158279295009,37.6460074219702,-12.6030529961857));
#27308=CARTESIAN_POINT('Ctrl Pts',(-4.90565273067089,37.51900742197,-14.6895517266055));
#27309=CARTESIAN_POINT('Ctrl Pts',(-2.45282636533548,37.3920074219702,-15.4865233241423));
#27310=CARTESIAN_POINT('Ctrl Pts',(-1.09153927723476E-18,37.26500742197,
-16.2834949216792));
#27311=CARTESIAN_POINT('Ctrl Pts',(2.45282636533548,37.1380074219702,-15.4865233241423));
#27312=CARTESIAN_POINT('Ctrl Pts',(4.90565273067095,37.0110074219701,-14.6895517266055));
#27313=CARTESIAN_POINT('Ctrl Pts',(6.4215827929502,36.8840074219702,-12.6030529961857));
#27314=CARTESIAN_POINT('Ctrl Pts',(7.93751285522931,36.7570074219701,-10.5165542657659));
#27315=CARTESIAN_POINT('Ctrl Pts',(7.93751285522939,36.6300074219701,-7.93750000000004));
#27316=CARTESIAN_POINT('Ctrl Pts',(7.93751285522937,36.5030074219699,-5.35844573423412));
#27317=CARTESIAN_POINT('Ctrl Pts',(6.4215827929502,36.37600742197,-3.27194700381427));
#27318=CARTESIAN_POINT('Ctrl Pts',(4.90565273067095,36.24900742197,-1.18544827339454));
#27319=CARTESIAN_POINT('Ctrl Pts',(2.45282636533548,36.12200742197,-0.388476675857653));
#27320=CARTESIAN_POINT('Ctrl Pts',(-5.4576963861738E-19,35.9950074219701,
0.408494921679244));
#27321=CARTESIAN_POINT('Ctrl Pts',(-2.45282636533542,35.86800742197,-0.388476675857653));
#27322=CARTESIAN_POINT('Ctrl Pts',(-4.90565273067089,35.7410074219701,-1.18544827339454));
#27323=CARTESIAN_POINT('Ctrl Pts',(-6.42158279295009,35.61400742197,-3.27194700381427));
#27324=CARTESIAN_POINT('Ctrl Pts',(-7.9375128552292,35.4870074219701,-5.35844573423412));
#27325=CARTESIAN_POINT('Ctrl Pts',(-7.93751285522927,35.3600074219701,-7.93750000000004));
#27326=CARTESIAN_POINT('Ctrl Pts',(-7.93751285522931,35.2330074219701,-10.5165542657659));
#27327=CARTESIAN_POINT('Ctrl Pts',(-6.42158279295003,35.1060074219702,-12.6030529961857));
#27328=CARTESIAN_POINT('Ctrl Pts',(-4.90565273067089,34.9790074219701,-14.6895517266055));
#27329=CARTESIAN_POINT('Ctrl Pts',(-2.45282636533548,34.8520074219702,-15.4865233241423));
#27330=CARTESIAN_POINT('Ctrl Pts',(0.,34.7250074219701,-16.2834949216792));
#27331=CARTESIAN_POINT('Ctrl Pts',(2.45282636533548,34.5980074219702,-15.4865233241423));
#27332=CARTESIAN_POINT('Ctrl Pts',(4.90565273067095,34.4710074219701,-14.6895517266055));
#27333=CARTESIAN_POINT('Ctrl Pts',(6.4215827929502,34.3440074219702,-12.6030529961857));
#27334=CARTESIAN_POINT('Ctrl Pts',(7.93751285522931,34.21700742197,-10.5165542657659));
#27335=CARTESIAN_POINT('Ctrl Pts',(7.93751285522939,34.0900074219701,-7.93750000000004));
#27336=CARTESIAN_POINT('Ctrl Pts',(7.93751285522926,33.9630074219701,-5.35844573423412));
#27337=CARTESIAN_POINT('Ctrl Pts',(6.4215827929502,33.8360074219702,-3.27194700381427));
#27338=CARTESIAN_POINT('Ctrl Pts',(4.90565273067095,33.7090074219701,-1.18544827339454));
#27339=CARTESIAN_POINT('Ctrl Pts',(2.45282636533548,33.5820074219701,-0.388476675857653));
#27340=CARTESIAN_POINT('Ctrl Pts',(0.,33.4550074219701,0.408494921679244));
#27341=CARTESIAN_POINT('Ctrl Pts',(-2.45282636533548,33.3280074219701,-0.388476675857653));
#27342=CARTESIAN_POINT('Ctrl Pts',(-4.90565273067095,33.20100742197,-1.18544827339454));
#27343=CARTESIAN_POINT('Ctrl Pts',(-6.42158279295003,33.07400742197,-3.27194700381427));
#27344=CARTESIAN_POINT('Ctrl Pts',(-7.93751285522931,32.9470074219701,-5.35844573423412));
#27345=CARTESIAN_POINT('Ctrl Pts',(-7.93751285522927,32.82000742197,-7.93750000000004));
#27346=CARTESIAN_POINT('Ctrl Pts',(-7.9375128552292,32.69300742197,-10.5165542657659));
#27347=CARTESIAN_POINT('Ctrl Pts',(-6.42158279295003,32.5660074219702,-12.6030529961857));
#27348=CARTESIAN_POINT('Ctrl Pts',(-4.90565273067089,32.4390074219701,-14.6895517266055));
#27349=CARTESIAN_POINT('Ctrl Pts',(-2.45282636533548,32.3120074219702,-15.4865233241423));
#27350=CARTESIAN_POINT('Ctrl Pts',(-1.16736848626568E-13,32.1850074219701,
-16.2834949216792));
#27351=CARTESIAN_POINT('Ctrl Pts',(2.45282636533548,32.0580074219702,-15.4865233241423));
#27352=CARTESIAN_POINT('Ctrl Pts',(4.90565273067083,31.9310074219701,-14.6895517266055));
#27353=CARTESIAN_POINT('Ctrl Pts',(6.4215827929502,31.8040074219701,-12.6030529961857));
#27354=CARTESIAN_POINT('Ctrl Pts',(7.93751285522931,31.67700742197,-10.5165542657659));
#27355=CARTESIAN_POINT('Ctrl Pts',(7.93751285522933,31.5500074219701,-7.93750000000004));
#27356=CARTESIAN_POINT('Ctrl Pts',(7.93751285522926,31.4230074219701,-5.35844573423412));
#27357=CARTESIAN_POINT('Ctrl Pts',(6.42158279295026,31.2960074219702,-3.27194700381427));
#27358=CARTESIAN_POINT('Ctrl Pts',(4.90565273067083,31.16900742197,-1.18544827339454));
#27359=CARTESIAN_POINT('Ctrl Pts',(2.45282636533548,31.04200742197,-0.388476675857653));
#27360=CARTESIAN_POINT('Ctrl Pts',(0.,30.9150074219701,0.408494921679244));
#27361=CARTESIAN_POINT('Ctrl Pts',(-2.45282636533548,30.7880074219701,-0.388476675857653));
#27362=CARTESIAN_POINT('Ctrl Pts',(-4.90565273067095,30.6610074219701,-1.18544827339454));
#27363=CARTESIAN_POINT('Ctrl Pts',(-6.42158279295003,30.53400742197,-3.27194700381427));
#27364=CARTESIAN_POINT('Ctrl Pts',(-7.93751285522926,30.40700742197,-5.35844573423412));
#27365=CARTESIAN_POINT('Ctrl Pts',(-7.93751285522922,30.28000742197,-7.93750000000004));
#27366=CARTESIAN_POINT('Ctrl Pts',(-7.93751285522931,30.15300742197,-10.5165542657659));
#27367=CARTESIAN_POINT('Ctrl Pts',(-6.42158279294998,30.0260074219701,-12.6030529961857));
#27368=CARTESIAN_POINT('Ctrl Pts',(-4.90565273067095,29.89900742197,-14.6895517266055));
#27369=CARTESIAN_POINT('Ctrl Pts',(-2.45282636533542,29.7720074219701,-15.4865233241423));
#27370=CARTESIAN_POINT('Ctrl Pts',(0.,29.64500742197,-16.2834949216792));
#27371=CARTESIAN_POINT('Ctrl Pts',(2.45282636533548,29.5180074219701,-15.4865233241423));
#27372=CARTESIAN_POINT('Ctrl Pts',(4.905652730671,29.3910074219701,-14.6895517266055));
#27373=CARTESIAN_POINT('Ctrl Pts',(6.4215827929502,29.2640074219701,-12.6030529961857));
#27374=CARTESIAN_POINT('Ctrl Pts',(7.93751285522931,29.1370074219701,-10.5165542657659));
#27375=CARTESIAN_POINT('Ctrl Pts',(7.93751285522922,29.0100074219701,-7.93750000000004));
#27376=CARTESIAN_POINT('Ctrl Pts',(7.93751285522931,28.88300742197,-5.35844573423412));
#27377=CARTESIAN_POINT('Ctrl Pts',(6.42158279295014,28.7560074219701,-3.27194700381427));
#27378=CARTESIAN_POINT('Ctrl Pts',(4.90565273067095,28.62900742197,-1.18544827339454));
#27379=CARTESIAN_POINT('Ctrl Pts',(2.45282636533548,28.5020074219701,-0.388476675857653));
#27380=CARTESIAN_POINT('Ctrl Pts',(1.16736848626568E-13,28.3750074219701,
0.408494921679244));
#27381=CARTESIAN_POINT('Ctrl Pts',(-2.45282636533548,28.2480074219701,-0.388476675857653));
#27382=CARTESIAN_POINT('Ctrl Pts',(-4.90565273067083,28.12100742197,-1.18544827339454));
#27383=CARTESIAN_POINT('Ctrl Pts',(-6.42158279294998,27.9940074219702,-3.27194700381427));
#27384=CARTESIAN_POINT('Ctrl Pts',(-7.93751285522926,27.8670074219701,-5.35844573423412));
#27385=CARTESIAN_POINT('Ctrl Pts',(-7.93751285522922,27.7400074219701,-7.93750000000004));
#27386=CARTESIAN_POINT('Ctrl Pts',(-7.93751285522931,27.6130074219701,-10.5165542657659));
#27387=CARTESIAN_POINT('Ctrl Pts',(-6.42158279295009,27.4860074219701,-12.6030529961857));
#27388=CARTESIAN_POINT('Ctrl Pts',(-4.90565273067083,27.35900742197,-14.6895517266055));
#27389=CARTESIAN_POINT('Ctrl Pts',(-2.45282636533542,27.2320074219702,-15.4865233241423));
#27390=CARTESIAN_POINT('Ctrl Pts',(1.16736848626568E-13,27.1050074219701,
-16.2834949216792));
#27391=CARTESIAN_POINT('Ctrl Pts',(2.45282636533548,26.9780074219701,-15.4865233241423));
#27392=CARTESIAN_POINT('Ctrl Pts',(4.90565273067089,26.8510074219701,-14.6895517266055));
#27393=CARTESIAN_POINT('Ctrl Pts',(6.42158279295014,26.7240074219702,-12.6030529961857));
#27394=CARTESIAN_POINT('Ctrl Pts',(7.93751285522926,26.59700742197,-10.5165542657659));
#27395=CARTESIAN_POINT('Ctrl Pts',(7.93751285522927,26.47000742197,-7.93750000000004));
#27396=CARTESIAN_POINT('Ctrl Pts',(7.93751285522931,26.3430074219701,-5.35844573423412));
#27397=CARTESIAN_POINT('Ctrl Pts',(6.4215827929502,26.2160074219701,-3.27194700381427));
#27398=CARTESIAN_POINT('Ctrl Pts',(4.905652730671,26.0890074219702,-1.18544827339454));
#27399=CARTESIAN_POINT('Ctrl Pts',(2.45282636533548,25.9620074219701,-0.388476675857653));
#27400=CARTESIAN_POINT('Ctrl Pts',(0.,25.8350074219701,0.408494921679244));
#27401=CARTESIAN_POINT('Ctrl Pts',(-2.45282636533548,25.7080074219701,-0.388476675857653));
#27402=CARTESIAN_POINT('Ctrl Pts',(-4.90565273067095,25.5810074219699,-1.18544827339454));
#27403=CARTESIAN_POINT('Ctrl Pts',(-6.42158279294998,25.4540074219701,-3.27194700381427));
#27404=CARTESIAN_POINT('Ctrl Pts',(-7.93751285522926,25.32700742197,-5.35844573423412));
#27405=CARTESIAN_POINT('Ctrl Pts',(-7.93751285522916,25.2000074219701,-7.93750000000004));
#27406=CARTESIAN_POINT('Ctrl Pts',(-7.93751285522931,25.07300742197,-10.5165542657659));
#27407=CARTESIAN_POINT('Ctrl Pts',(-6.42158279295009,24.9460074219701,-12.6030529961857));
#27408=CARTESIAN_POINT('Ctrl Pts',(-4.90565273067095,24.8190074219701,-14.6895517266055));
#27409=CARTESIAN_POINT('Ctrl Pts',(-2.45282636533537,24.6920074219702,-15.4865233241423));
#27410=CARTESIAN_POINT('Ctrl Pts',(0.,24.56500742197,-16.2834949216792));
#27411=CARTESIAN_POINT('Ctrl Pts',(2.45282636533548,24.4380074219702,-15.4865233241423));
#27412=CARTESIAN_POINT('Ctrl Pts',(4.90565273067089,24.3110074219699,-14.6895517266055));
#27413=CARTESIAN_POINT('Ctrl Pts',(6.42158279295003,24.1840074219703,-12.6030529961857));
#27414=CARTESIAN_POINT('Ctrl Pts',(7.93751285522937,24.05700742197,-10.5165542657659));
#27415=CARTESIAN_POINT('Ctrl Pts',(7.93751285522927,23.9300074219701,-7.93750000000004));
#27416=CARTESIAN_POINT('Ctrl Pts',(7.9375128552292,23.80300742197,-5.35844573423412));
#27417=CARTESIAN_POINT('Ctrl Pts',(6.42158279295009,23.6760074219701,-3.27194700381427));
#27418=CARTESIAN_POINT('Ctrl Pts',(4.90565273067089,23.5490074219701,-1.18544827339454));
#27419=CARTESIAN_POINT('Ctrl Pts',(2.45282636533553,23.4220074219701,-0.388476675857653));
#27420=CARTESIAN_POINT('Ctrl Pts',(1.09153927723476E-18,23.29500742197,
0.408494921679244));
#27421=CARTESIAN_POINT('Ctrl Pts',(-2.45282636533542,23.1680074219701,-0.388476675857653));
#27422=CARTESIAN_POINT('Ctrl Pts',(-4.90565273067095,23.0410074219701,-1.18544827339454));
#27423=CARTESIAN_POINT('Ctrl Pts',(-6.42158279295009,22.9140074219701,-3.27194700381427));
#27424=CARTESIAN_POINT('Ctrl Pts',(-7.93751285522931,22.78700742197,-5.35844573423412));
#27425=CARTESIAN_POINT('Ctrl Pts',(-7.93751285522927,22.6600074219701,-7.93750000000004));
#27426=CARTESIAN_POINT('Ctrl Pts',(-7.93751285522926,22.53300742197,-10.5165542657659));
#27427=CARTESIAN_POINT('Ctrl Pts',(-6.42158279295009,22.4060074219703,-12.6030529961857));
#27428=CARTESIAN_POINT('Ctrl Pts',(-4.90565273067095,22.27900742197,-14.6895517266055));
#27429=CARTESIAN_POINT('Ctrl Pts',(-2.45282636533548,22.1520074219702,-15.4865233241423));
#27430=CARTESIAN_POINT('Ctrl Pts',(0.,22.02500742197,-16.2834949216792));
#27431=CARTESIAN_POINT('Ctrl Pts',(2.45282636533548,21.8980074219703,-15.4865233241423));
#27432=CARTESIAN_POINT('Ctrl Pts',(4.90565273067095,21.77100742197,-14.6895517266055));
#27433=CARTESIAN_POINT('Ctrl Pts',(6.42158279295009,21.6440074219702,-12.6030529961857));
#27434=CARTESIAN_POINT('Ctrl Pts',(7.93751285522926,21.5170074219701,-10.5165542657659));
#27435=CARTESIAN_POINT('Ctrl Pts',(7.93751285522927,21.3900074219701,-7.93750000000004));
#27436=CARTESIAN_POINT('Ctrl Pts',(7.93751285522931,21.26300742197,-5.35844573423412));
#27437=CARTESIAN_POINT('Ctrl Pts',(6.42158279295009,21.13600742197,-3.27194700381427));
#27438=CARTESIAN_POINT('Ctrl Pts',(5.62930008354685,21.0696323914868,-2.18146340668965));
#27439=CARTESIAN_POINT('Ctrl Pts',(4.52145020702022,20.9998588479374,-1.41365156886918));
#27440=CARTESIAN_POINT('Ctrl Pts',(0.0471929759279855,20.7180654494099,
1.68729896628553));
#27441=CARTESIAN_POINT('Ctrl Pts',(-4.42706425516419,20.4362720508822,4.78824950144024));
#27442=CARTESIAN_POINT('Ctrl Pts',(6.56268467749999,20.5962500034686,-7.93750000000004));
#27443=CARTESIAN_POINT('Ctrl Pts',(6.56268467749997,20.4692500034686,-5.80515448811441));
#27444=CARTESIAN_POINT('Ctrl Pts',(5.3093234328217,20.3422500034686,-4.08005073111972));
#27445=CARTESIAN_POINT('Ctrl Pts',(4.65426916952368,20.2758749724933,-3.1784458861888));
#27446=CARTESIAN_POINT('Ctrl Pts',(3.7383059945976,20.2061014284303,-2.54362398482789));
#27447=CARTESIAN_POINT('Origin',(-2.53888687851145E-9,74.888750003468,-7.9374999999999));
#27448=CARTESIAN_POINT('Ctrl Pts',(6.56268467749999,19.9612500034686,-7.93750000000004));
#27449=CARTESIAN_POINT('Ctrl Pts',(6.56268467750003,19.8342500034686,-5.80515448811441));
#27450=CARTESIAN_POINT('Ctrl Pts',(5.30932343282159,19.7072500034685,-4.08005073111972));
#27451=CARTESIAN_POINT('Ctrl Pts',(4.6542690872318,19.6408749641548,-3.17844577292378));
#27452=CARTESIAN_POINT('Ctrl Pts',(3.73830577091051,19.5711014113908,-2.54362382979823));
#27453=CARTESIAN_POINT('Ctrl Pts',(-7.93749999999999,73.7775000069372,-7.93749999999999));
#27454=CARTESIAN_POINT('Ctrl Pts',(-7.93749999999997,73.6505000069372,-10.5165500888487));
#27455=CARTESIAN_POINT('Ctrl Pts',(-6.42157239285113,73.5235000069373,-12.6030454400715));
#27456=CARTESIAN_POINT('Ctrl Pts',(-4.90564478570226,73.3965000069372,-14.6895407912943));
#27457=CARTESIAN_POINT('Ctrl Pts',(-2.45282239285111,73.2695000069373,-15.4865110980928));
#27458=CARTESIAN_POINT('Ctrl Pts',(0.,73.1425000069373,-16.2834814048913));
#27459=CARTESIAN_POINT('Ctrl Pts',(2.45282239285127,73.0155000069373,-15.4865110980928));
#27460=CARTESIAN_POINT('Ctrl Pts',(4.90564478570231,72.8885000069371,-14.6895407912943));
#27461=CARTESIAN_POINT('Ctrl Pts',(6.42157239285118,72.7615000069373,-12.6030454400715));
#27462=CARTESIAN_POINT('Ctrl Pts',(7.93750000000003,72.6345000069371,-10.5165500888487));
#27463=CARTESIAN_POINT('Ctrl Pts',(7.9375000000001,72.5075000069372,-7.93749999999999));
#27464=CARTESIAN_POINT('Ctrl Pts',(7.93749999999997,72.3805000069372,-5.35844991115131));
#27465=CARTESIAN_POINT('Ctrl Pts',(6.42157239285124,72.2535000069372,-3.27195455992851));
#27466=CARTESIAN_POINT('Ctrl Pts',(4.90564478570231,72.1265000069371,-1.18545920870573));
#27467=CARTESIAN_POINT('Ctrl Pts',(2.45282239285116,71.9995000069372,-0.38848890190718));
#27468=CARTESIAN_POINT('Ctrl Pts',(0.,71.8725000069372,0.408481404891264));
#27469=CARTESIAN_POINT('Ctrl Pts',(-2.45282239285105,71.7455000069372,-0.38848890190718));
#27470=CARTESIAN_POINT('Ctrl Pts',(-4.90564478570226,71.6185000069372,-1.18545920870573));
#27471=CARTESIAN_POINT('Ctrl Pts',(-6.42157239285113,71.4915000069372,-3.2719545599284));
#27472=CARTESIAN_POINT('Ctrl Pts',(-7.93750000000003,71.3645000069373,-5.35844991115131));
#27473=CARTESIAN_POINT('Ctrl Pts',(-7.93749999999999,71.2375000069373,-7.93749999999999));
#27474=CARTESIAN_POINT('Ctrl Pts',(-7.93750000000003,71.1105000069372,-10.5165500888487));
#27475=CARTESIAN_POINT('Ctrl Pts',(-6.42157239285113,70.9835000069373,-12.6030454400715));
#27476=CARTESIAN_POINT('Ctrl Pts',(-4.90564478570226,70.8565000069373,-14.6895407912943));
#27477=CARTESIAN_POINT('Ctrl Pts',(-2.45282239285105,70.7295000069373,-15.4865110980928));
#27478=CARTESIAN_POINT('Ctrl Pts',(0.,70.6025000069372,-16.2834814048913));
#27479=CARTESIAN_POINT('Ctrl Pts',(2.45282239285127,70.4755000069374,-15.4865110980928));
#27480=CARTESIAN_POINT('Ctrl Pts',(4.90564478570231,70.3485000069372,-14.6895407912943));
#27481=CARTESIAN_POINT('Ctrl Pts',(6.42157239285118,70.2215000069373,-12.6030454400715));
#27482=CARTESIAN_POINT('Ctrl Pts',(7.93750000000003,70.0945000069371,-10.5165500888487));
#27483=CARTESIAN_POINT('Ctrl Pts',(7.9375000000001,69.9675000069372,-7.93749999999999));
#27484=CARTESIAN_POINT('Ctrl Pts',(7.93749999999997,69.8405000069372,-5.35844991115131));
#27485=CARTESIAN_POINT('Ctrl Pts',(6.42157239285124,69.7135000069371,-3.27195455992851));
#27486=CARTESIAN_POINT('Ctrl Pts',(4.90564478570231,69.5865000069372,-1.18545920870573));
#27487=CARTESIAN_POINT('Ctrl Pts',(2.45282239285122,69.4595000069373,-0.38848890190718));
#27488=CARTESIAN_POINT('Ctrl Pts',(-5.83678785436452E-14,69.3325000069372,
0.408481404891264));
#27489=CARTESIAN_POINT('Ctrl Pts',(-2.45282239285111,69.2055000069372,-0.38848890190718));
#27490=CARTESIAN_POINT('Ctrl Pts',(-4.90564478570231,69.0785000069372,-1.18545920870573));
#27491=CARTESIAN_POINT('Ctrl Pts',(-6.42157239285113,68.9515000069372,-3.2719545599284));
#27492=CARTESIAN_POINT('Ctrl Pts',(-7.93750000000003,68.8245000069372,-5.35844991115131));
#27493=CARTESIAN_POINT('Ctrl Pts',(-7.93749999999999,68.6975000069372,-7.93749999999999));
#27494=CARTESIAN_POINT('Ctrl Pts',(-7.93749999999991,68.5705000069372,-10.5165500888487));
#27495=CARTESIAN_POINT('Ctrl Pts',(-6.42157239285113,68.4435000069374,-12.6030454400715));
#27496=CARTESIAN_POINT('Ctrl Pts',(-4.90564478570231,68.3165000069372,-14.6895407912943));
#27497=CARTESIAN_POINT('Ctrl Pts',(-2.45282239285116,68.1895000069373,-15.4865110980928));
#27498=CARTESIAN_POINT('Ctrl Pts',(-1.1673575708729E-13,68.0625000069372,
-16.2834814048913));
#27499=CARTESIAN_POINT('Ctrl Pts',(2.45282239285116,67.9355000069373,-15.4865110980928));
#27500=CARTESIAN_POINT('Ctrl Pts',(4.90564478570231,67.8085000069373,-14.6895407912943));
#27501=CARTESIAN_POINT('Ctrl Pts',(6.42157239285124,67.6815000069373,-12.6030454400715));
#27502=CARTESIAN_POINT('Ctrl Pts',(7.93750000000003,67.5545000069373,-10.5165500888487));
#27503=CARTESIAN_POINT('Ctrl Pts',(7.93749999999999,67.4275000069372,-7.93749999999999));
#27504=CARTESIAN_POINT('Ctrl Pts',(7.93750000000009,67.3005000069372,-5.35844991115131));
#27505=CARTESIAN_POINT('Ctrl Pts',(6.42157239285113,67.1735000069372,-3.27195455992851));
#27506=CARTESIAN_POINT('Ctrl Pts',(4.9056447857022,67.0465000069371,-1.18545920870573));
#27507=CARTESIAN_POINT('Ctrl Pts',(2.45282239285116,66.9195000069373,-0.38848890190718));
#27508=CARTESIAN_POINT('Ctrl Pts',(5.83678785436452E-14,66.7925000069371,
0.408481404891264));
#27509=CARTESIAN_POINT('Ctrl Pts',(-2.45282239285122,66.6655000069371,-0.38848890190718));
#27510=CARTESIAN_POINT('Ctrl Pts',(-4.9056447857022,66.5385000069372,-1.18545920870573));
#27511=CARTESIAN_POINT('Ctrl Pts',(-6.42157239285113,66.4115000069373,-3.2719545599284));
#27512=CARTESIAN_POINT('Ctrl Pts',(-7.93749999999997,66.2845000069373,-5.35844991115131));
#27513=CARTESIAN_POINT('Ctrl Pts',(-7.93749999999999,66.1575000069372,-7.93749999999999));
#27514=CARTESIAN_POINT('Ctrl Pts',(-7.93750000000003,66.0305000069372,-10.5165500888487));
#27515=CARTESIAN_POINT('Ctrl Pts',(-6.42157239285107,65.9035000069373,-12.6030454400715));
#27516=CARTESIAN_POINT('Ctrl Pts',(-4.9056447857022,65.7765000069371,-14.6895407912943));
#27517=CARTESIAN_POINT('Ctrl Pts',(-2.45282239285116,65.6495000069373,-15.4865110980928));
#27518=CARTESIAN_POINT('Ctrl Pts',(1.1673575708729E-13,65.5225000069372,
-16.2834814048913));
#27519=CARTESIAN_POINT('Ctrl Pts',(2.45282239285105,65.3955000069373,-15.4865110980928));
#27520=CARTESIAN_POINT('Ctrl Pts',(4.90564478570237,65.2685000069372,-14.6895407912943));
#27521=CARTESIAN_POINT('Ctrl Pts',(6.42157239285124,65.1415000069373,-12.6030454400715));
#27522=CARTESIAN_POINT('Ctrl Pts',(7.93749999999991,65.0145000069372,-10.5165500888487));
#27523=CARTESIAN_POINT('Ctrl Pts',(7.93749999999999,64.8875000069373,-7.93749999999999));
#27524=CARTESIAN_POINT('Ctrl Pts',(7.93750000000003,64.7605000069372,-5.35844991115131));
#27525=CARTESIAN_POINT('Ctrl Pts',(6.42157239285113,64.6335000069372,-3.2719545599284));
#27526=CARTESIAN_POINT('Ctrl Pts',(4.90564478570231,64.5065000069371,-1.18545920870573));
#27527=CARTESIAN_POINT('Ctrl Pts',(2.45282239285116,64.3795000069372,-0.38848890190718));
#27528=CARTESIAN_POINT('Ctrl Pts',(1.1673575708729E-13,64.2525000069372,
0.408481404891264));
#27529=CARTESIAN_POINT('Ctrl Pts',(-2.45282239285116,64.1255000069372,-0.38848890190718));
#27530=CARTESIAN_POINT('Ctrl Pts',(-4.90564478570231,63.9985000069371,-1.18545920870573));
#27531=CARTESIAN_POINT('Ctrl Pts',(-6.42157239285107,63.8715000069372,-3.2719545599284));
#27532=CARTESIAN_POINT('Ctrl Pts',(-7.93749999999997,63.7445000069372,-5.35844991115131));
#27533=CARTESIAN_POINT('Ctrl Pts',(-7.93749999999999,63.6175000069372,-7.93749999999999));
#27534=CARTESIAN_POINT('Ctrl Pts',(-7.93750000000003,63.4905000069372,-10.5165500888487));
#27535=CARTESIAN_POINT('Ctrl Pts',(-6.42157239285118,63.3635000069373,-12.6030454400715));
#27536=CARTESIAN_POINT('Ctrl Pts',(-4.9056447857022,63.2365000069372,-14.6895407912943));
#27537=CARTESIAN_POINT('Ctrl Pts',(-2.45282239285116,63.1095000069373,-15.4865110980928));
#27538=CARTESIAN_POINT('Ctrl Pts',(0.,62.9825000069372,-16.2834814048913));
#27539=CARTESIAN_POINT('Ctrl Pts',(2.45282239285111,62.8555000069373,-15.4865110980928));
#27540=CARTESIAN_POINT('Ctrl Pts',(4.90564478570226,62.7285000069371,-14.6895407912943));
#27541=CARTESIAN_POINT('Ctrl Pts',(6.42157239285113,62.6015000069373,-12.6030454400715));
#27542=CARTESIAN_POINT('Ctrl Pts',(7.93750000000003,62.4745000069372,-10.5165500888487));
#27543=CARTESIAN_POINT('Ctrl Pts',(7.93750000000004,62.3475000069372,-7.93749999999999));
#27544=CARTESIAN_POINT('Ctrl Pts',(7.93750000000003,62.2205000069372,-5.35844991115131));
#27545=CARTESIAN_POINT('Ctrl Pts',(6.42157239285118,62.0935000069373,-3.2719545599284));
#27546=CARTESIAN_POINT('Ctrl Pts',(4.90564478570226,61.9665000069372,-1.18545920870573));
#27547=CARTESIAN_POINT('Ctrl Pts',(2.45282239285116,61.8395000069372,-0.38848890190718));
#27548=CARTESIAN_POINT('Ctrl Pts',(0.,61.7125000069371,0.408481404891264));
#27549=CARTESIAN_POINT('Ctrl Pts',(-2.45282239285116,61.5855000069373,-0.38848890190718));
#27550=CARTESIAN_POINT('Ctrl Pts',(-4.90564478570231,61.4585000069373,-1.18545920870573));
#27551=CARTESIAN_POINT('Ctrl Pts',(-6.42157239285113,61.3315000069372,-3.2719545599284));
#27552=CARTESIAN_POINT('Ctrl Pts',(-7.93749999999997,61.2045000069371,-5.35844991115131));
#27553=CARTESIAN_POINT('Ctrl Pts',(-7.93749999999993,61.0775000069371,-7.93749999999999));
#27554=CARTESIAN_POINT('Ctrl Pts',(-7.93750000000003,60.9505000069371,-10.5165500888487));
#27555=CARTESIAN_POINT('Ctrl Pts',(-6.42157239285113,60.8235000069373,-12.6030454400715));
#27556=CARTESIAN_POINT('Ctrl Pts',(-4.90564478570231,60.6965000069371,-14.6895407912943));
#27557=CARTESIAN_POINT('Ctrl Pts',(-2.45282239285111,60.5695000069374,-15.4865110980928));
#27558=CARTESIAN_POINT('Ctrl Pts',(0.,60.4425000069371,-16.2834814048913));
#27559=CARTESIAN_POINT('Ctrl Pts',(2.45282239285116,60.3155000069373,-15.4865110980928));
#27560=CARTESIAN_POINT('Ctrl Pts',(4.90564478570237,60.1885000069372,-14.6895407912943));
#27561=CARTESIAN_POINT('Ctrl Pts',(6.42157239285113,60.0615000069373,-12.6030454400715));
#27562=CARTESIAN_POINT('Ctrl Pts',(7.93749999999997,59.9345000069372,-10.5165500888487));
#27563=CARTESIAN_POINT('Ctrl Pts',(7.93750000000004,59.8075000069372,-7.93749999999999));
#27564=CARTESIAN_POINT('Ctrl Pts',(7.93750000000003,59.6805000069371,-5.35844991115131));
#27565=CARTESIAN_POINT('Ctrl Pts',(6.42157239285118,59.5535000069372,-3.2719545599284));
#27566=CARTESIAN_POINT('Ctrl Pts',(4.90564478570226,59.4265000069372,-1.18545920870573));
#27567=CARTESIAN_POINT('Ctrl Pts',(2.45282239285116,59.2995000069371,-0.38848890190718));
#27568=CARTESIAN_POINT('Ctrl Pts',(1.1673575708729E-13,59.1725000069372,
0.408481404891264));
#27569=CARTESIAN_POINT('Ctrl Pts',(-2.45282239285116,59.0455000069372,-0.38848890190718));
#27570=CARTESIAN_POINT('Ctrl Pts',(-4.90564478570231,58.9185000069372,-1.18545920870573));
#27571=CARTESIAN_POINT('Ctrl Pts',(-6.42157239285113,58.7915000069372,-3.2719545599284));
#27572=CARTESIAN_POINT('Ctrl Pts',(-7.93750000000003,58.6645000069372,-5.35844991115131));
#27573=CARTESIAN_POINT('Ctrl Pts',(-7.93750000000004,58.5375000069372,-7.93749999999999));
#27574=CARTESIAN_POINT('Ctrl Pts',(-7.93749999999997,58.4105000069373,-10.5165500888487));
#27575=CARTESIAN_POINT('Ctrl Pts',(-6.42157239285113,58.2835000069372,-12.6030454400715));
#27576=CARTESIAN_POINT('Ctrl Pts',(-4.90564478570231,58.1565000069371,-14.6895407912943));
#27577=CARTESIAN_POINT('Ctrl Pts',(-2.45282239285122,58.0295000069373,-15.4865110980928));
#27578=CARTESIAN_POINT('Ctrl Pts',(5.83678785436452E-14,57.9025000069372,
-16.2834814048913));
#27579=CARTESIAN_POINT('Ctrl Pts',(2.45282239285116,57.7755000069372,-15.4865110980928));
#27580=CARTESIAN_POINT('Ctrl Pts',(4.90564478570231,57.6485000069371,-14.6895407912943));
#27581=CARTESIAN_POINT('Ctrl Pts',(6.42157239285118,57.5215000069373,-12.6030454400715));
#27582=CARTESIAN_POINT('Ctrl Pts',(7.93749999999997,57.3945000069372,-10.5165500888487));
#27583=CARTESIAN_POINT('Ctrl Pts',(7.9375000000001,57.2675000069372,-7.93749999999999));
#27584=CARTESIAN_POINT('Ctrl Pts',(7.93750000000003,57.1405000069372,-5.35844991115131));
#27585=CARTESIAN_POINT('Ctrl Pts',(6.42157239285124,57.0135000069372,-3.2719545599284));
#27586=CARTESIAN_POINT('Ctrl Pts',(4.90564478570237,56.8865000069372,-1.18545920870573));
#27587=CARTESIAN_POINT('Ctrl Pts',(2.45282239285105,56.7595000069371,-0.38848890190718));
#27588=CARTESIAN_POINT('Ctrl Pts',(0.,56.6325000069371,0.408481404891264));
#27589=CARTESIAN_POINT('Ctrl Pts',(-2.45282239285116,56.5055000069372,-0.38848890190718));
#27590=CARTESIAN_POINT('Ctrl Pts',(-4.90564478570226,56.3785000069372,-1.18545920870573));
#27591=CARTESIAN_POINT('Ctrl Pts',(-6.42157239285113,56.2515000069372,-3.2719545599284));
#27592=CARTESIAN_POINT('Ctrl Pts',(-7.93749999999991,56.1245000069371,-5.35844991115131));
#27593=CARTESIAN_POINT('Ctrl Pts',(-7.93749999999999,55.9975000069372,-7.93749999999999));
#27594=CARTESIAN_POINT('Ctrl Pts',(-7.93749999999997,55.8705000069372,-10.5165500888487));
#27595=CARTESIAN_POINT('Ctrl Pts',(-6.42157239285113,55.7435000069373,-12.6030454400715));
#27596=CARTESIAN_POINT('Ctrl Pts',(-4.90564478570231,55.6165000069373,-14.6895407912943));
#27597=CARTESIAN_POINT('Ctrl Pts',(-2.45282239285116,55.4895000069373,-15.4865110980928));
#27598=CARTESIAN_POINT('Ctrl Pts',(0.,55.3625000069372,-16.2834814048913));
#27599=CARTESIAN_POINT('Ctrl Pts',(2.45282239285116,55.2355000069373,-15.4865110980928));
#27600=CARTESIAN_POINT('Ctrl Pts',(4.90564478570231,55.1085000069371,-14.6895407912943));
#27601=CARTESIAN_POINT('Ctrl Pts',(6.42157239285118,54.9815000069373,-12.6030454400715));
#27602=CARTESIAN_POINT('Ctrl Pts',(7.93750000000009,54.8545000069371,-10.5165500888487));
#27603=CARTESIAN_POINT('Ctrl Pts',(7.9375000000001,54.7275000069372,-7.93750000000004));
#27604=CARTESIAN_POINT('Ctrl Pts',(7.93749999999991,54.6005000069371,-5.35844991115131));
#27605=CARTESIAN_POINT('Ctrl Pts',(6.42157239285124,54.4735000069372,-3.27195455992846));
#27606=CARTESIAN_POINT('Ctrl Pts',(4.90564478570231,54.3465000069372,-1.18545920870573));
#27607=CARTESIAN_POINT('Ctrl Pts',(2.45282239285111,54.2195000069373,-0.388488901907236));
#27608=CARTESIAN_POINT('Ctrl Pts',(0.,54.0925000069371,0.408481404891264));
#27609=CARTESIAN_POINT('Ctrl Pts',(-2.45282239285111,53.9655000069372,-0.388488901907236));
#27610=CARTESIAN_POINT('Ctrl Pts',(-4.90564478570226,53.8385000069372,-1.18545920870573));
#27611=CARTESIAN_POINT('Ctrl Pts',(-6.42157239285113,53.7115000069372,-3.27195455992846));
#27612=CARTESIAN_POINT('Ctrl Pts',(-7.93750000000003,53.5845000069372,-5.35844991115131));
#27613=CARTESIAN_POINT('Ctrl Pts',(-7.93749999999999,53.4575000069372,-7.93750000000004));
#27614=CARTESIAN_POINT('Ctrl Pts',(-7.93749999999997,53.3305000069372,-10.5165500888487));
#27615=CARTESIAN_POINT('Ctrl Pts',(-6.42157239285113,53.2035000069373,-12.6030454400715));
#27616=CARTESIAN_POINT('Ctrl Pts',(-4.90564478570231,53.0765000069372,-14.6895407912943));
#27617=CARTESIAN_POINT('Ctrl Pts',(-2.45282239285116,52.9495000069372,-15.4865110980928));
#27618=CARTESIAN_POINT('Ctrl Pts',(0.,52.8225000069372,-16.2834814048913));
#27619=CARTESIAN_POINT('Ctrl Pts',(2.45282239285116,52.6955000069374,-15.4865110980928));
#27620=CARTESIAN_POINT('Ctrl Pts',(4.90564478570231,52.5685000069372,-14.6895407912943));
#27621=CARTESIAN_POINT('Ctrl Pts',(6.42157239285124,52.4415000069373,-12.6030454400715));
#27622=CARTESIAN_POINT('Ctrl Pts',(7.93749999999997,52.3145000069372,-10.5165500888487));
#27623=CARTESIAN_POINT('Ctrl Pts',(7.9375000000001,52.1875000069372,-7.93750000000004));
#27624=CARTESIAN_POINT('Ctrl Pts',(7.93750000000009,52.0605000069371,-5.35844991115131));
#27625=CARTESIAN_POINT('Ctrl Pts',(6.42157239285124,51.9335000069372,-3.27195455992846));
#27626=CARTESIAN_POINT('Ctrl Pts',(4.90564478570231,51.8065000069371,-1.18545920870573));
#27627=CARTESIAN_POINT('Ctrl Pts',(2.45282239285116,51.6795000069372,-0.388488901907236));
#27628=CARTESIAN_POINT('Ctrl Pts',(0.,51.5525000069372,0.408481404891264));
#27629=CARTESIAN_POINT('Ctrl Pts',(-2.45282239285122,51.4255000069372,-0.388488901907236));
#27630=CARTESIAN_POINT('Ctrl Pts',(-4.90564478570226,51.2985000069372,-1.18545920870573));
#27631=CARTESIAN_POINT('Ctrl Pts',(-6.42157239285113,51.1715000069372,-3.27195455992846));
#27632=CARTESIAN_POINT('Ctrl Pts',(-7.93750000000003,51.0445000069372,-5.35844991115131));
#27633=CARTESIAN_POINT('Ctrl Pts',(-7.93749999999999,50.9175000069372,-7.93750000000004));
#27634=CARTESIAN_POINT('Ctrl Pts',(-7.93749999999997,50.7905000069372,-10.5165500888487));
#27635=CARTESIAN_POINT('Ctrl Pts',(-6.42157239285107,50.6635000069373,-12.6030454400715));
#27636=CARTESIAN_POINT('Ctrl Pts',(-4.90564478570237,50.5365000069371,-14.6895407912943));
#27637=CARTESIAN_POINT('Ctrl Pts',(-2.45282239285116,50.4095000069373,-15.4865110980928));
#27638=CARTESIAN_POINT('Ctrl Pts',(0.,50.2825000069372,-16.2834814048913));
#27639=CARTESIAN_POINT('Ctrl Pts',(2.45282239285105,50.1555000069373,-15.4865110980928));
#27640=CARTESIAN_POINT('Ctrl Pts',(4.90564478570231,50.0285000069372,-14.6895407912943));
#27641=CARTESIAN_POINT('Ctrl Pts',(6.42157239285124,49.9015000069373,-12.6030454400715));
#27642=CARTESIAN_POINT('Ctrl Pts',(7.93750000000003,49.7745000069372,-10.5165500888487));
#27643=CARTESIAN_POINT('Ctrl Pts',(7.93749999999999,49.6475000069372,-7.93750000000004));
#27644=CARTESIAN_POINT('Ctrl Pts',(7.93750000000009,49.5205000069372,-5.35844991115131));
#27645=CARTESIAN_POINT('Ctrl Pts',(6.42157239285113,49.3935000069372,-3.27195455992846));
#27646=CARTESIAN_POINT('Ctrl Pts',(4.90564478570231,49.2665000069372,-1.18545920870573));
#27647=CARTESIAN_POINT('Ctrl Pts',(2.45282239285116,49.1395000069372,-0.388488901907236));
#27648=CARTESIAN_POINT('Ctrl Pts',(0.,49.0125000069372,0.408481404891264));
#27649=CARTESIAN_POINT('Ctrl Pts',(-2.45282239285116,48.8855000069372,-0.388488901907236));
#27650=CARTESIAN_POINT('Ctrl Pts',(-4.90564478570226,48.7585000069371,-1.18545920870573));
#27651=CARTESIAN_POINT('Ctrl Pts',(-6.42157239285107,48.6315000069372,-3.27195455992846));
#27652=CARTESIAN_POINT('Ctrl Pts',(-7.93750000000003,48.5045000069372,-5.35844991115131));
#27653=CARTESIAN_POINT('Ctrl Pts',(-7.93749999999999,48.3775000069372,-7.93750000000004));
#27654=CARTESIAN_POINT('Ctrl Pts',(-7.93750000000003,48.2505000069372,-10.5165500888487));
#27655=CARTESIAN_POINT('Ctrl Pts',(-6.42157239285107,48.1235000069373,-12.6030454400715));
#27656=CARTESIAN_POINT('Ctrl Pts',(-4.90564478570226,47.9965000069372,-14.6895407912943));
#27657=CARTESIAN_POINT('Ctrl Pts',(-2.45282239285116,47.8695000069373,-15.4865110980928));
#27658=CARTESIAN_POINT('Ctrl Pts',(0.,47.7425000069372,-16.2834814048913));
#27659=CARTESIAN_POINT('Ctrl Pts',(2.45282239285111,47.6155000069373,-15.4865110980928));
#27660=CARTESIAN_POINT('Ctrl Pts',(4.90564478570231,47.4885000069371,-14.6895407912943));
#27661=CARTESIAN_POINT('Ctrl Pts',(6.42157239285113,47.3615000069373,-12.6030454400715));
#27662=CARTESIAN_POINT('Ctrl Pts',(7.93750000000003,47.2345000069372,-10.5165500888487));
#27663=CARTESIAN_POINT('Ctrl Pts',(7.93750000000004,47.1075000069372,-7.93750000000004));
#27664=CARTESIAN_POINT('Ctrl Pts',(7.93749999999997,46.9805000069371,-5.35844991115131));
#27665=CARTESIAN_POINT('Ctrl Pts',(6.42157239285118,46.8535000069372,-3.27195455992846));
#27666=CARTESIAN_POINT('Ctrl Pts',(4.90564478570231,46.7265000069371,-1.18545920870573));
#27667=CARTESIAN_POINT('Ctrl Pts',(2.45282239285116,46.5995000069372,-0.388488901907236));
#27668=CARTESIAN_POINT('Ctrl Pts',(-5.83678785436452E-14,46.4725000069372,
0.408481404891264));
#27669=CARTESIAN_POINT('Ctrl Pts',(-2.45282239285116,46.3455000069373,-0.388488901907236));
#27670=CARTESIAN_POINT('Ctrl Pts',(-4.90564478570231,46.2185000069372,-1.18545920870573));
#27671=CARTESIAN_POINT('Ctrl Pts',(-6.42157239285107,46.0915000069372,-3.27195455992846));
#27672=CARTESIAN_POINT('Ctrl Pts',(-7.93749999999997,45.9645000069371,-5.35844991115131));
#27673=CARTESIAN_POINT('Ctrl Pts',(-7.93749999999993,45.8375000069371,-7.93750000000004));
#27674=CARTESIAN_POINT('Ctrl Pts',(-7.93749999999991,45.7105000069371,-10.5165500888487));
#27675=CARTESIAN_POINT('Ctrl Pts',(-6.42157239285113,45.5835000069373,-12.6030454400715));
#27676=CARTESIAN_POINT('Ctrl Pts',(-4.90564478570231,45.4565000069371,-14.6895407912943));
#27677=CARTESIAN_POINT('Ctrl Pts',(-2.45282239285111,45.3295000069374,-15.4865110980928));
#27678=CARTESIAN_POINT('Ctrl Pts',(-5.83678785436452E-14,45.2025000069371,
-16.2834814048912));
#27679=CARTESIAN_POINT('Ctrl Pts',(2.45282239285116,45.0755000069373,-15.4865110980928));
#27680=CARTESIAN_POINT('Ctrl Pts',(4.90564478570237,44.9485000069372,-14.6895407912943));
#27681=CARTESIAN_POINT('Ctrl Pts',(6.42157239285113,44.8215000069374,-12.6030454400715));
#27682=CARTESIAN_POINT('Ctrl Pts',(7.93750000000003,44.6945000069372,-10.5165500888487));
#27683=CARTESIAN_POINT('Ctrl Pts',(7.93750000000004,44.5675000069372,-7.93750000000004));
#27684=CARTESIAN_POINT('Ctrl Pts',(7.93750000000009,44.4405000069371,-5.35844991115131));
#27685=CARTESIAN_POINT('Ctrl Pts',(6.42157239285118,44.3135000069372,-3.27195455992846));
#27686=CARTESIAN_POINT('Ctrl Pts',(4.9056447857022,44.1865000069372,-1.18545920870573));
#27687=CARTESIAN_POINT('Ctrl Pts',(2.45282239285116,44.0595000069372,-0.388488901907236));
#27688=CARTESIAN_POINT('Ctrl Pts',(0.,43.9325000069372,0.408481404891264));
#27689=CARTESIAN_POINT('Ctrl Pts',(-2.45282239285116,43.8055000069373,-0.388488901907236));
#27690=CARTESIAN_POINT('Ctrl Pts',(-4.9056447857022,43.6785000069372,-1.18545920870573));
#27691=CARTESIAN_POINT('Ctrl Pts',(-6.42157239285113,43.5515000069372,-3.27195455992846));
#27692=CARTESIAN_POINT('Ctrl Pts',(-7.93749999999997,43.4245000069372,-5.35844991115131));
#27693=CARTESIAN_POINT('Ctrl Pts',(-7.93749999999993,43.2975000069372,-7.93750000000004));
#27694=CARTESIAN_POINT('Ctrl Pts',(-7.93750000000003,43.1705000069372,-10.5165500888487));
#27695=CARTESIAN_POINT('Ctrl Pts',(-6.42157239285113,43.0435000069372,-12.6030454400715));
#27696=CARTESIAN_POINT('Ctrl Pts',(-4.90564478570231,42.9165000069372,-14.6895407912943));
#27697=CARTESIAN_POINT('Ctrl Pts',(-2.45282239285116,42.7895000069373,-15.4865110980928));
#27698=CARTESIAN_POINT('Ctrl Pts',(1.1673575708729E-13,42.6625000069372,
-16.2834814048912));
#27699=CARTESIAN_POINT('Ctrl Pts',(2.45282239285116,42.5355000069372,-15.4865110980928));
#27700=CARTESIAN_POINT('Ctrl Pts',(4.90564478570237,42.4085000069371,-14.6895407912943));
#27701=CARTESIAN_POINT('Ctrl Pts',(6.42157239285118,42.2815000069373,-12.6030454400715));
#27702=CARTESIAN_POINT('Ctrl Pts',(7.93749999999991,42.1545000069372,-10.5165500888487));
#27703=CARTESIAN_POINT('Ctrl Pts',(7.9375000000001,42.0275000069373,-7.93750000000004));
#27704=CARTESIAN_POINT('Ctrl Pts',(7.93750000000003,41.9005000069372,-5.35844991115131));
#27705=CARTESIAN_POINT('Ctrl Pts',(6.42157239285124,41.7735000069372,-3.27195455992846));
#27706=CARTESIAN_POINT('Ctrl Pts',(4.90564478570231,41.6465000069372,-1.18545920870573));
#27707=CARTESIAN_POINT('Ctrl Pts',(2.45282239285105,41.5195000069371,-0.388488901907236));
#27708=CARTESIAN_POINT('Ctrl Pts',(1.1673575708729E-13,41.3925000069372,
0.408481404891264));
#27709=CARTESIAN_POINT('Ctrl Pts',(-2.45282239285116,41.2655000069372,-0.388488901907236));
#27710=CARTESIAN_POINT('Ctrl Pts',(-4.90564478570231,41.1385000069372,-1.18545920870573));
#27711=CARTESIAN_POINT('Ctrl Pts',(-6.42157239285113,41.0115000069372,-3.27195455992846));
#27712=CARTESIAN_POINT('Ctrl Pts',(-7.93749999999997,40.8845000069371,-5.35844991115131));
#27713=CARTESIAN_POINT('Ctrl Pts',(-7.93749999999999,40.7575000069372,-7.93750000000004));
#27714=CARTESIAN_POINT('Ctrl Pts',(-7.93750000000003,40.6305000069372,-10.5165500888487));
#27715=CARTESIAN_POINT('Ctrl Pts',(-6.42157239285113,40.5035000069373,-12.6030454400715));
#27716=CARTESIAN_POINT('Ctrl Pts',(-4.9056447857022,40.3765000069371,-14.6895407912943));
#27717=CARTESIAN_POINT('Ctrl Pts',(-2.45282239285116,40.2495000069373,-15.4865110980928));
#27718=CARTESIAN_POINT('Ctrl Pts',(0.,40.1225000069371,-16.2834814048912));
#27719=CARTESIAN_POINT('Ctrl Pts',(2.45282239285116,39.9955000069373,-15.4865110980928));
#27720=CARTESIAN_POINT('Ctrl Pts',(4.90564478570226,39.868500006937,-14.6895407912943));
#27721=CARTESIAN_POINT('Ctrl Pts',(6.42157239285118,39.7415000069373,-12.6030454400715));
#27722=CARTESIAN_POINT('Ctrl Pts',(7.93750000000009,39.6145000069371,-10.5165500888487));
#27723=CARTESIAN_POINT('Ctrl Pts',(7.9375000000001,39.4875000069372,-7.93750000000004));
#27724=CARTESIAN_POINT('Ctrl Pts',(7.93750000000003,39.3605000069371,-5.35844991115131));
#27725=CARTESIAN_POINT('Ctrl Pts',(6.42157239285124,39.2335000069372,-3.27195455992846));
#27726=CARTESIAN_POINT('Ctrl Pts',(4.90564478570226,39.1065000069372,-1.18545920870573));
#27727=CARTESIAN_POINT('Ctrl Pts',(2.45282239285111,38.9795000069372,-0.388488901907236));
#27728=CARTESIAN_POINT('Ctrl Pts',(0.,38.8525000069371,0.408481404891264));
#27729=CARTESIAN_POINT('Ctrl Pts',(-2.45282239285111,38.7255000069372,-0.388488901907236));
#27730=CARTESIAN_POINT('Ctrl Pts',(-4.90564478570231,38.5985000069372,-1.18545920870573));
#27731=CARTESIAN_POINT('Ctrl Pts',(-6.42157239285113,38.4715000069372,-3.27195455992846));
#27732=CARTESIAN_POINT('Ctrl Pts',(-7.93749999999997,38.3445000069371,-5.35844991115131));
#27733=CARTESIAN_POINT('Ctrl Pts',(-7.93749999999999,38.2175000069373,-7.93750000000004));
#27734=CARTESIAN_POINT('Ctrl Pts',(-7.93750000000003,38.0905000069372,-10.5165500888487));
#27735=CARTESIAN_POINT('Ctrl Pts',(-6.42157239285113,37.9635000069373,-12.6030454400715));
#27736=CARTESIAN_POINT('Ctrl Pts',(-4.90564478570231,37.8365000069372,-14.6895407912943));
#27737=CARTESIAN_POINT('Ctrl Pts',(-2.45282239285116,37.7095000069373,-15.4865110980927));
#27738=CARTESIAN_POINT('Ctrl Pts',(0.,37.5825000069371,-16.2834814048912));
#27739=CARTESIAN_POINT('Ctrl Pts',(2.45282239285116,37.4555000069374,-15.4865110980927));
#27740=CARTESIAN_POINT('Ctrl Pts',(4.90564478570237,37.3285000069371,-14.6895407912943));
#27741=CARTESIAN_POINT('Ctrl Pts',(6.42157239285124,37.2015000069372,-12.6030454400715));
#27742=CARTESIAN_POINT('Ctrl Pts',(7.93750000000009,37.0745000069372,-10.5165500888487));
#27743=CARTESIAN_POINT('Ctrl Pts',(7.9375000000001,36.9475000069372,-7.93750000000004));
#27744=CARTESIAN_POINT('Ctrl Pts',(7.93750000000003,36.8205000069372,-5.35844991115131));
#27745=CARTESIAN_POINT('Ctrl Pts',(6.42157239285124,36.6935000069371,-3.27195455992846));
#27746=CARTESIAN_POINT('Ctrl Pts',(4.90564478570226,36.5665000069371,-1.18545920870573));
#27747=CARTESIAN_POINT('Ctrl Pts',(2.45282239285116,36.4395000069373,-0.388488901907236));
#27748=CARTESIAN_POINT('Ctrl Pts',(0.,36.3125000069372,0.408481404891264));
#27749=CARTESIAN_POINT('Ctrl Pts',(-2.45282239285111,36.1855000069372,-0.388488901907236));
#27750=CARTESIAN_POINT('Ctrl Pts',(-4.90564478570231,36.0585000069371,-1.18545920870573));
#27751=CARTESIAN_POINT('Ctrl Pts',(-6.42157239285113,35.9315000069372,-3.27195455992846));
#27752=CARTESIAN_POINT('Ctrl Pts',(-7.93750000000003,35.8045000069372,-5.35844991115131));
#27753=CARTESIAN_POINT('Ctrl Pts',(-7.93749999999999,35.6775000069372,-7.93750000000004));
#27754=CARTESIAN_POINT('Ctrl Pts',(-7.93749999999997,35.5505000069372,-10.5165500888487));
#27755=CARTESIAN_POINT('Ctrl Pts',(-6.42157239285107,35.4235000069373,-12.6030454400715));
#27756=CARTESIAN_POINT('Ctrl Pts',(-4.90564478570231,35.2965000069372,-14.6895407912943));
#27757=CARTESIAN_POINT('Ctrl Pts',(-2.45282239285116,35.1695000069372,-15.4865110980927));
#27758=CARTESIAN_POINT('Ctrl Pts',(1.1673575708729E-13,35.0425000069372,
-16.2834814048912));
#27759=CARTESIAN_POINT('Ctrl Pts',(2.45282239285116,34.9155000069373,-15.4865110980927));
#27760=CARTESIAN_POINT('Ctrl Pts',(4.90564478570231,34.7885000069371,-14.6895407912943));
#27761=CARTESIAN_POINT('Ctrl Pts',(6.42157239285124,34.6615000069373,-12.6030454400715));
#27762=CARTESIAN_POINT('Ctrl Pts',(7.93749999999997,34.5345000069371,-10.5165500888487));
#27763=CARTESIAN_POINT('Ctrl Pts',(7.93750000000004,34.4075000069372,-7.93750000000004));
#27764=CARTESIAN_POINT('Ctrl Pts',(7.93750000000003,34.2805000069372,-5.35844991115131));
#27765=CARTESIAN_POINT('Ctrl Pts',(6.42157239285124,34.1535000069372,-3.27195455992846));
#27766=CARTESIAN_POINT('Ctrl Pts',(4.90564478570237,34.0265000069372,-1.18545920870573));
#27767=CARTESIAN_POINT('Ctrl Pts',(2.45282239285116,33.8995000069372,-0.388488901907236));
#27768=CARTESIAN_POINT('Ctrl Pts',(0.,33.7725000069372,0.408481404891264));
#27769=CARTESIAN_POINT('Ctrl Pts',(-2.45282239285116,33.6455000069371,-0.388488901907236));
#27770=CARTESIAN_POINT('Ctrl Pts',(-4.90564478570226,33.5185000069371,-1.18545920870573));
#27771=CARTESIAN_POINT('Ctrl Pts',(-6.42157239285107,33.3915000069372,-3.27195455992846));
#27772=CARTESIAN_POINT('Ctrl Pts',(-7.93749999999991,33.2645000069372,-5.35844991115131));
#27773=CARTESIAN_POINT('Ctrl Pts',(-7.93749999999999,33.1375000069372,-7.93750000000004));
#27774=CARTESIAN_POINT('Ctrl Pts',(-7.93749999999997,33.0105000069372,-10.5165500888487));
#27775=CARTESIAN_POINT('Ctrl Pts',(-6.42157239285107,32.8835000069373,-12.6030454400715));
#27776=CARTESIAN_POINT('Ctrl Pts',(-4.90564478570231,32.7565000069372,-14.6895407912943));
#27777=CARTESIAN_POINT('Ctrl Pts',(-2.45282239285116,32.6295000069373,-15.4865110980927));
#27778=CARTESIAN_POINT('Ctrl Pts',(0.,32.5025000069372,-16.2834814048912));
#27779=CARTESIAN_POINT('Ctrl Pts',(2.45282239285111,32.3755000069373,-15.4865110980927));
#27780=CARTESIAN_POINT('Ctrl Pts',(4.90564478570231,32.2485000069372,-14.6895407912943));
#27781=CARTESIAN_POINT('Ctrl Pts',(6.42157239285124,32.1215000069373,-12.6030454400715));
#27782=CARTESIAN_POINT('Ctrl Pts',(7.93750000000009,31.9945000069372,-10.5165500888487));
#27783=CARTESIAN_POINT('Ctrl Pts',(7.93750000000004,31.8675000069372,-7.93750000000004));
#27784=CARTESIAN_POINT('Ctrl Pts',(7.93749999999991,31.7405000069372,-5.35844991115131));
#27785=CARTESIAN_POINT('Ctrl Pts',(6.42157239285118,31.6135000069372,-3.27195455992846));
#27786=CARTESIAN_POINT('Ctrl Pts',(4.90564478570231,31.4865000069371,-1.18545920870573));
#27787=CARTESIAN_POINT('Ctrl Pts',(2.45282239285116,31.3595000069372,-0.388488901907236));
#27788=CARTESIAN_POINT('Ctrl Pts',(0.,31.2325000069371,0.408481404891264));
#27789=CARTESIAN_POINT('Ctrl Pts',(-2.45282239285116,31.1055000069372,-0.388488901907236));
#27790=CARTESIAN_POINT('Ctrl Pts',(-4.90564478570226,30.9785000069371,-1.18545920870573));
#27791=CARTESIAN_POINT('Ctrl Pts',(-6.42157239285107,30.8515000069372,-3.27195455992846));
#27792=CARTESIAN_POINT('Ctrl Pts',(-7.93750000000003,30.7245000069372,-5.35844991115131));
#27793=CARTESIAN_POINT('Ctrl Pts',(-7.93749999999993,30.5975000069372,-7.93750000000004));
#27794=CARTESIAN_POINT('Ctrl Pts',(-7.93749999999997,30.4705000069371,-10.5165500888487));
#27795=CARTESIAN_POINT('Ctrl Pts',(-6.42157239285107,30.3435000069373,-12.6030454400715));
#27796=CARTESIAN_POINT('Ctrl Pts',(-4.90564478570226,30.2165000069371,-14.6895407912943));
#27797=CARTESIAN_POINT('Ctrl Pts',(-2.45282239285111,30.0895000069373,-15.4865110980927));
#27798=CARTESIAN_POINT('Ctrl Pts',(0.,29.9625000069372,-16.2834814048912));
#27799=CARTESIAN_POINT('Ctrl Pts',(2.45282239285116,29.8355000069373,-15.4865110980927));
#27800=CARTESIAN_POINT('Ctrl Pts',(4.9056447857022,29.7085000069372,-14.6895407912943));
#27801=CARTESIAN_POINT('Ctrl Pts',(6.42157239285113,29.5815000069373,-12.6030454400715));
#27802=CARTESIAN_POINT('Ctrl Pts',(7.93750000000003,29.4545000069372,-10.5165500888487));
#27803=CARTESIAN_POINT('Ctrl Pts',(7.9375000000001,29.3275000069372,-7.93750000000004));
#27804=CARTESIAN_POINT('Ctrl Pts',(7.93750000000009,29.2005000069372,-5.35844991115131));
#27805=CARTESIAN_POINT('Ctrl Pts',(6.42157239285118,29.0735000069372,-3.27195455992846));
#27806=CARTESIAN_POINT('Ctrl Pts',(4.90564478570231,28.9465000069371,-1.18545920870573));
#27807=CARTESIAN_POINT('Ctrl Pts',(2.45282239285116,28.8195000069372,-0.388488901907236));
#27808=CARTESIAN_POINT('Ctrl Pts',(-1.1673575708729E-13,28.6925000069372,
0.408481404891264));
#27809=CARTESIAN_POINT('Ctrl Pts',(-2.45282239285116,28.5655000069372,-0.388488901907236));
#27810=CARTESIAN_POINT('Ctrl Pts',(-4.90564478570237,28.4385000069371,-1.18545920870573));
#27811=CARTESIAN_POINT('Ctrl Pts',(-6.42157239285102,28.3115000069372,-3.27195455992846));
#27812=CARTESIAN_POINT('Ctrl Pts',(-7.93750000000003,28.1845000069372,-5.35844991115131));
#27813=CARTESIAN_POINT('Ctrl Pts',(-7.93749999999988,28.0575000069372,-7.93750000000004));
#27814=CARTESIAN_POINT('Ctrl Pts',(-7.93749999999997,27.9305000069372,-10.5165500888487));
#27815=CARTESIAN_POINT('Ctrl Pts',(-6.42157239285113,27.8035000069373,-12.6030454400715));
#27816=CARTESIAN_POINT('Ctrl Pts',(-4.90564478570237,27.6765000069372,-14.6895407912943));
#27817=CARTESIAN_POINT('Ctrl Pts',(-2.45282239285111,27.5495000069373,-15.4865110980927));
#27818=CARTESIAN_POINT('Ctrl Pts',(0.,27.4225000069372,-16.2834814048912));
#27819=CARTESIAN_POINT('Ctrl Pts',(2.45282239285116,27.2955000069372,-15.4865110980927));
#27820=CARTESIAN_POINT('Ctrl Pts',(4.90564478570231,27.1685000069371,-14.6895407912943));
#27821=CARTESIAN_POINT('Ctrl Pts',(6.42157239285118,27.0415000069373,-12.6030454400715));
#27822=CARTESIAN_POINT('Ctrl Pts',(7.93750000000003,26.9145000069372,-10.5165500888487));
#27823=CARTESIAN_POINT('Ctrl Pts',(7.9375000000001,26.7875000069372,-7.93750000000004));
#27824=CARTESIAN_POINT('Ctrl Pts',(7.93750000000009,26.6605000069372,-5.35844991115131));
#27825=CARTESIAN_POINT('Ctrl Pts',(6.42157239285124,26.5335000069372,-3.27195455992846));
#27826=CARTESIAN_POINT('Ctrl Pts',(4.90564478570231,26.4065000069372,-1.18545920870573));
#27827=CARTESIAN_POINT('Ctrl Pts',(2.45282239285122,26.2795000069371,-0.388488901907236));
#27828=CARTESIAN_POINT('Ctrl Pts',(0.,26.1525000069371,0.408481404891264));
#27829=CARTESIAN_POINT('Ctrl Pts',(-2.45282239285116,26.0255000069372,-0.388488901907236));
#27830=CARTESIAN_POINT('Ctrl Pts',(-4.9056447857022,25.8985000069372,-1.18545920870573));
#27831=CARTESIAN_POINT('Ctrl Pts',(-6.42157239285113,25.7715000069371,-3.27195455992846));
#27832=CARTESIAN_POINT('Ctrl Pts',(-7.93750000000003,25.6445000069371,-5.35844991115131));
#27833=CARTESIAN_POINT('Ctrl Pts',(-7.93749999999999,25.5175000069372,-7.93750000000004));
#27834=CARTESIAN_POINT('Ctrl Pts',(-7.93750000000003,25.3905000069371,-10.5165500888487));
#27835=CARTESIAN_POINT('Ctrl Pts',(-6.42157239285113,25.2635000069372,-12.6030454400715));
#27836=CARTESIAN_POINT('Ctrl Pts',(-4.90564478570226,25.1365000069371,-14.6895407912943));
#27837=CARTESIAN_POINT('Ctrl Pts',(-2.45282239285116,25.0095000069373,-15.4865110980927));
#27838=CARTESIAN_POINT('Ctrl Pts',(0.,24.8825000069371,-16.2834814048912));
#27839=CARTESIAN_POINT('Ctrl Pts',(2.45282239285116,24.7555000069373,-15.4865110980927));
#27840=CARTESIAN_POINT('Ctrl Pts',(4.90564478570231,24.6285000069372,-14.6895407912943));
#27841=CARTESIAN_POINT('Ctrl Pts',(6.42157239285124,24.5015000069373,-12.6030454400715));
#27842=CARTESIAN_POINT('Ctrl Pts',(7.93750000000003,24.3745000069371,-10.5165500888487));
#27843=CARTESIAN_POINT('Ctrl Pts',(7.9375000000001,24.2475000069372,-7.93750000000004));
#27844=CARTESIAN_POINT('Ctrl Pts',(7.93749999999997,24.1205000069371,-5.35844991115131));
#27845=CARTESIAN_POINT('Ctrl Pts',(6.42157239285124,23.9935000069372,-3.27195455992846));
#27846=CARTESIAN_POINT('Ctrl Pts',(4.90564478570231,23.8665000069372,-1.18545920870573));
#27847=CARTESIAN_POINT('Ctrl Pts',(2.45282239285111,23.7395000069371,-0.388488901907236));
#27848=CARTESIAN_POINT('Ctrl Pts',(0.,23.612500006937,0.408481404891264));
#27849=CARTESIAN_POINT('Ctrl Pts',(-2.45282239285111,23.4855000069372,-0.388488901907236));
#27850=CARTESIAN_POINT('Ctrl Pts',(-4.90564478570231,23.3585000069372,-1.18545920870573));
#27851=CARTESIAN_POINT('Ctrl Pts',(-6.42157239285113,23.2315000069372,-3.27195455992846));
#27852=CARTESIAN_POINT('Ctrl Pts',(-7.93749999999997,23.1045000069372,-5.35844991115131));
#27853=CARTESIAN_POINT('Ctrl Pts',(-7.93749999999999,22.9775000069372,-7.93750000000004));
#27854=CARTESIAN_POINT('Ctrl Pts',(-7.93749999999991,22.8505000069371,-10.5165500888487));
#27855=CARTESIAN_POINT('Ctrl Pts',(-6.42157239285113,22.7235000069373,-12.6030454400715));
#27856=CARTESIAN_POINT('Ctrl Pts',(-4.9056447857022,22.5965000069371,-14.6895407912943));
#27857=CARTESIAN_POINT('Ctrl Pts',(-2.45282239285116,22.4695000069373,-15.4865110980927));
#27858=CARTESIAN_POINT('Ctrl Pts',(0.,22.3425000069372,-16.2834814048912));
#27859=CARTESIAN_POINT('Ctrl Pts',(2.45282239285116,22.2155000069373,-15.4865110980927));
#27860=CARTESIAN_POINT('Ctrl Pts',(4.90564478570226,22.0885000069371,-14.6895407912943));
#27861=CARTESIAN_POINT('Ctrl Pts',(6.42157239285124,21.9615000069372,-12.6030454400715));
#27862=CARTESIAN_POINT('Ctrl Pts',(7.93750000000003,21.8345000069372,-10.5165500888487));
#27863=CARTESIAN_POINT('Ctrl Pts',(7.93749999999999,21.7075000069372,-7.93750000000004));
#27864=CARTESIAN_POINT('Ctrl Pts',(7.93750000000014,21.5805000069372,-5.35844991115131));
#27865=CARTESIAN_POINT('Ctrl Pts',(6.42157239285124,21.4535000069371,-3.27195455992846));
#27866=CARTESIAN_POINT('Ctrl Pts',(4.9056447857022,21.3265000069371,-1.18545920870573));
#27867=CARTESIAN_POINT('Ctrl Pts',(2.45282239285116,21.1995000069373,-0.388488901907236));
#27868=CARTESIAN_POINT('Ctrl Pts',(0.,21.0725000069371,0.408481404891264));
#27869=CARTESIAN_POINT('Ctrl Pts',(-2.45282239285111,20.9455000069371,-0.388488901907236));
#27870=CARTESIAN_POINT('Ctrl Pts',(-4.90564478570231,20.8185000069372,-1.18545920870573));
#27871=CARTESIAN_POINT('Ctrl Pts',(-6.42157239285113,20.6915000069372,-3.27195455992846));
#27872=CARTESIAN_POINT('Ctrl Pts',(-7.93749999999997,20.5645000069371,-5.35844991115131));
#27873=CARTESIAN_POINT('Ctrl Pts',(-7.93749999999999,20.4375000069372,-7.93750000000004));
#27874=CARTESIAN_POINT('Ctrl Pts',(-7.93750000000003,20.3105000069372,-10.5165500888487));
#27875=CARTESIAN_POINT('Ctrl Pts',(-6.42157239285107,20.1835000069373,-12.6030454400715));
#27876=CARTESIAN_POINT('Ctrl Pts',(-4.90564478570231,20.0565000069372,-14.6895407912943));
#27877=CARTESIAN_POINT('Ctrl Pts',(-2.45282239285116,19.9295000069372,-15.4865110980927));
#27878=CARTESIAN_POINT('Ctrl Pts',(1.1673575708729E-13,19.8025000069371,
-16.2834814048912));
#27879=CARTESIAN_POINT('Ctrl Pts',(2.45282239285122,19.6755000069374,-15.4865110980927));
#27880=CARTESIAN_POINT('Ctrl Pts',(4.90564478570237,19.5485000069371,-14.6895407912943));
#27881=CARTESIAN_POINT('Ctrl Pts',(6.42157239285124,19.4215000069373,-12.6030454400715));
#27882=CARTESIAN_POINT('Ctrl Pts',(7.93749999999991,19.2945000069371,-10.5165500888487));
#27883=CARTESIAN_POINT('Ctrl Pts',(7.93749999999999,19.1675000069371,-7.93750000000004));
#27884=CARTESIAN_POINT('Ctrl Pts',(7.93750000000003,19.0405000069371,-5.35844991115131));
#27885=CARTESIAN_POINT('Ctrl Pts',(6.42157239285124,18.9135000069372,-3.27195455992846));
#27886=CARTESIAN_POINT('Ctrl Pts',(5.62929016097025,18.8471249089612,-2.18147162005691));
#27887=CARTESIAN_POINT('Ctrl Pts',(4.52144069443246,18.7773512949848,-1.41366061688136));
#27888=CARTESIAN_POINT('Ctrl Pts',(-6.56268467750004,74.5712500034686,-7.93749999999999));
#27889=CARTESIAN_POINT('Ctrl Pts',(-6.56268467750003,74.4442500034686,-10.0698455118856));
#27890=CARTESIAN_POINT('Ctrl Pts',(-5.30932343282159,74.3172500034687,-11.7949492688802));
#27891=CARTESIAN_POINT('Ctrl Pts',(-4.05596218814306,74.1902500034686,-13.5200530258749));
#27892=CARTESIAN_POINT('Ctrl Pts',(-2.02798109407148,74.0632500034687,-14.1789840269267));
#27893=CARTESIAN_POINT('Ctrl Pts',(1.1673575708729E-13,73.9362500034685,
-14.8379150279786));
#27894=CARTESIAN_POINT('Ctrl Pts',(2.0279810940716,73.8092500034687,-14.1789840269267));
#27895=CARTESIAN_POINT('Ctrl Pts',(4.05596218814324,73.6822500034687,-13.5200530258749));
#27896=CARTESIAN_POINT('Ctrl Pts',(5.30932343282159,73.5552500034686,-11.7949492688802));
#27897=CARTESIAN_POINT('Ctrl Pts',(6.56268467750003,73.4282500034686,-10.0698455118856));
#27898=CARTESIAN_POINT('Ctrl Pts',(6.5626846775001,73.3012500034686,-7.93749999999999));
#27899=CARTESIAN_POINT('Ctrl Pts',(6.56268467750003,73.1742500034686,-5.80515448811441));
#27900=CARTESIAN_POINT('Ctrl Pts',(5.30932343282164,73.0472500034686,-4.08005073111967));
#27901=CARTESIAN_POINT('Ctrl Pts',(4.05596218814318,72.9202500034686,-2.35494697412514));
#27902=CARTESIAN_POINT('Ctrl Pts',(2.02798109407154,72.7932500034686,-1.69601597307328));
#27903=CARTESIAN_POINT('Ctrl Pts',(1.1673575708729E-13,72.6662500034686,
-1.0370849720215));
#27904=CARTESIAN_POINT('Ctrl Pts',(-2.02798109407165,72.5392500034687,-1.69601597307328));
#27905=CARTESIAN_POINT('Ctrl Pts',(-4.05596218814312,72.4122500034686,-2.35494697412514));
#27906=CARTESIAN_POINT('Ctrl Pts',(-5.30932343282153,72.2852500034685,-4.08005073111967));
#27907=CARTESIAN_POINT('Ctrl Pts',(-6.56268467750008,72.1582500034687,-5.80515448811441));
#27908=CARTESIAN_POINT('Ctrl Pts',(-6.56268467750004,72.0312500034686,-7.93749999999999));
#27909=CARTESIAN_POINT('Ctrl Pts',(-6.56268467750003,71.9042500034686,-10.0698455118856));
#27910=CARTESIAN_POINT('Ctrl Pts',(-5.30932343282159,71.7772500034686,-11.7949492688802));
#27911=CARTESIAN_POINT('Ctrl Pts',(-4.05596218814318,71.6502500034686,-13.5200530258749));
#27912=CARTESIAN_POINT('Ctrl Pts',(-2.0279810940716,71.5232500034686,-14.1789840269267));
#27913=CARTESIAN_POINT('Ctrl Pts',(0.,71.3962500034686,-14.8379150279786));
#27914=CARTESIAN_POINT('Ctrl Pts',(2.02798109407165,71.2692500034687,-14.1789840269267));
#27915=CARTESIAN_POINT('Ctrl Pts',(4.05596218814312,71.1422500034685,-13.5200530258749));
#27916=CARTESIAN_POINT('Ctrl Pts',(5.30932343282159,71.0152500034686,-11.7949492688802));
#27917=CARTESIAN_POINT('Ctrl Pts',(6.56268467750003,70.8882500034686,-10.0698455118856));
#27918=CARTESIAN_POINT('Ctrl Pts',(6.56268467749999,70.7612500034687,-7.93749999999999));
#27919=CARTESIAN_POINT('Ctrl Pts',(6.56268467750003,70.6342500034686,-5.80515448811441));
#27920=CARTESIAN_POINT('Ctrl Pts',(5.30932343282164,70.5072500034686,-4.08005073111967));
#27921=CARTESIAN_POINT('Ctrl Pts',(4.05596218814324,70.3802500034686,-2.35494697412514));
#27922=CARTESIAN_POINT('Ctrl Pts',(2.0279810940716,70.2532500034686,-1.69601597307328));
#27923=CARTESIAN_POINT('Ctrl Pts',(0.,70.1262500034686,-1.0370849720215));
#27924=CARTESIAN_POINT('Ctrl Pts',(-2.0279810940716,69.9992500034686,-1.69601597307328));
#27925=CARTESIAN_POINT('Ctrl Pts',(-4.05596218814312,69.8722500034686,-2.35494697412514));
#27926=CARTESIAN_POINT('Ctrl Pts',(-5.30932343282159,69.7452500034687,-4.08005073111967));
#27927=CARTESIAN_POINT('Ctrl Pts',(-6.56268467749997,69.6182500034686,-5.80515448811441));
#27928=CARTESIAN_POINT('Ctrl Pts',(-6.56268467749999,69.4912500034686,-7.93749999999999));
#27929=CARTESIAN_POINT('Ctrl Pts',(-6.56268467749997,69.3642500034686,-10.0698455118856));
#27930=CARTESIAN_POINT('Ctrl Pts',(-5.30932343282153,69.2372500034686,-11.7949492688802));
#27931=CARTESIAN_POINT('Ctrl Pts',(-4.05596218814312,69.1102500034686,-13.5200530258749));
#27932=CARTESIAN_POINT('Ctrl Pts',(-2.02798109407154,68.9832500034687,-14.1789840269267));
#27933=CARTESIAN_POINT('Ctrl Pts',(0.,68.8562500034686,-14.8379150279786));
#27934=CARTESIAN_POINT('Ctrl Pts',(2.02798109407165,68.7292500034686,-14.1789840269267));
#27935=CARTESIAN_POINT('Ctrl Pts',(4.05596218814312,68.6022500034686,-13.5200530258749));
#27936=CARTESIAN_POINT('Ctrl Pts',(5.30932343282164,68.4752500034687,-11.7949492688802));
#27937=CARTESIAN_POINT('Ctrl Pts',(6.56268467749997,68.3482500034685,-10.0698455118856));
#27938=CARTESIAN_POINT('Ctrl Pts',(6.56268467749999,68.2212500034686,-7.93749999999999));
#27939=CARTESIAN_POINT('Ctrl Pts',(6.56268467750003,68.0942500034685,-5.80515448811441));
#27940=CARTESIAN_POINT('Ctrl Pts',(5.3093234328217,67.9672500034686,-4.08005073111967));
#27941=CARTESIAN_POINT('Ctrl Pts',(4.05596218814312,67.8402500034685,-2.35494697412514));
#27942=CARTESIAN_POINT('Ctrl Pts',(2.0279810940716,67.7132500034686,-1.69601597307328));
#27943=CARTESIAN_POINT('Ctrl Pts',(1.1673575708729E-13,67.5862500034684,
-1.0370849720215));
#27944=CARTESIAN_POINT('Ctrl Pts',(-2.0279810940716,67.4592500034686,-1.69601597307328));
#27945=CARTESIAN_POINT('Ctrl Pts',(-4.05596218814312,67.3322500034685,-2.35494697412514));
#27946=CARTESIAN_POINT('Ctrl Pts',(-5.30932343282153,67.2052500034686,-4.08005073111967));
#27947=CARTESIAN_POINT('Ctrl Pts',(-6.56268467750003,67.0782500034685,-5.80515448811441));
#27948=CARTESIAN_POINT('Ctrl Pts',(-6.56268467749999,66.9512500034686,-7.93749999999999));
#27949=CARTESIAN_POINT('Ctrl Pts',(-6.56268467749997,66.8242500034685,-10.0698455118856));
#27950=CARTESIAN_POINT('Ctrl Pts',(-5.30932343282153,66.6972500034686,-11.7949492688802));
#27951=CARTESIAN_POINT('Ctrl Pts',(-4.05596218814312,66.5702500034686,-13.5200530258749));
#27952=CARTESIAN_POINT('Ctrl Pts',(-2.02798109407165,66.4432500034688,-14.1789840269267));
#27953=CARTESIAN_POINT('Ctrl Pts',(0.,66.3162500034685,-14.8379150279786));
#27954=CARTESIAN_POINT('Ctrl Pts',(2.02798109407154,66.1892500034688,-14.1789840269267));
#27955=CARTESIAN_POINT('Ctrl Pts',(4.05596218814312,66.0622500034686,-13.5200530258749));
#27956=CARTESIAN_POINT('Ctrl Pts',(5.30932343282164,65.9352500034686,-11.7949492688802));
#27957=CARTESIAN_POINT('Ctrl Pts',(6.56268467750008,65.8082500034686,-10.0698455118856));
#27958=CARTESIAN_POINT('Ctrl Pts',(6.56268467749999,65.6812500034686,-7.93749999999999));
#27959=CARTESIAN_POINT('Ctrl Pts',(6.56268467749991,65.5542500034687,-5.80515448811441));
#27960=CARTESIAN_POINT('Ctrl Pts',(5.3093234328217,65.4272500034686,-4.08005073111967));
#27961=CARTESIAN_POINT('Ctrl Pts',(4.05596218814324,65.3002500034687,-2.35494697412514));
#27962=CARTESIAN_POINT('Ctrl Pts',(2.0279810940716,65.1732500034686,-1.69601597307328));
#27963=CARTESIAN_POINT('Ctrl Pts',(0.,65.0462500034686,-1.0370849720215));
#27964=CARTESIAN_POINT('Ctrl Pts',(-2.0279810940716,64.9192500034686,-1.69601597307328));
#27965=CARTESIAN_POINT('Ctrl Pts',(-4.05596218814312,64.7922500034686,-2.35494697412514));
#27966=CARTESIAN_POINT('Ctrl Pts',(-5.30932343282153,64.6652500034686,-4.08005073111967));
#27967=CARTESIAN_POINT('Ctrl Pts',(-6.56268467750003,64.5382500034686,-5.80515448811441));
#27968=CARTESIAN_POINT('Ctrl Pts',(-6.56268467749999,64.4112500034687,-7.93749999999999));
#27969=CARTESIAN_POINT('Ctrl Pts',(-6.56268467749997,64.2842500034685,-10.0698455118856));
#27970=CARTESIAN_POINT('Ctrl Pts',(-5.30932343282148,64.1572500034686,-11.7949492688802));
#27971=CARTESIAN_POINT('Ctrl Pts',(-4.05596218814312,64.0302500034686,-13.5200530258749));
#27972=CARTESIAN_POINT('Ctrl Pts',(-2.02798109407165,63.9032500034688,-14.1789840269267));
#27973=CARTESIAN_POINT('Ctrl Pts',(0.,63.7762500034686,-14.8379150279786));
#27974=CARTESIAN_POINT('Ctrl Pts',(2.0279810940716,63.6492500034688,-14.1789840269267));
#27975=CARTESIAN_POINT('Ctrl Pts',(4.05596218814312,63.5222500034685,-13.5200530258749));
#27976=CARTESIAN_POINT('Ctrl Pts',(5.3093234328217,63.3952500034686,-11.7949492688802));
#27977=CARTESIAN_POINT('Ctrl Pts',(6.56268467749997,63.2682500034685,-10.0698455118856));
#27978=CARTESIAN_POINT('Ctrl Pts',(6.56268467750004,63.1412500034686,-7.93749999999999));
#27979=CARTESIAN_POINT('Ctrl Pts',(6.56268467750003,63.0142500034686,-5.80515448811441));
#27980=CARTESIAN_POINT('Ctrl Pts',(5.30932343282164,62.8872500034686,-4.08005073111967));
#27981=CARTESIAN_POINT('Ctrl Pts',(4.05596218814312,62.7602500034686,-2.35494697412514));
#27982=CARTESIAN_POINT('Ctrl Pts',(2.02798109407165,62.6332500034686,-1.69601597307328));
#27983=CARTESIAN_POINT('Ctrl Pts',(0.,62.5062500034686,-1.0370849720215));
#27984=CARTESIAN_POINT('Ctrl Pts',(-2.02798109407154,62.3792500034686,-1.69601597307328));
#27985=CARTESIAN_POINT('Ctrl Pts',(-4.05596218814324,62.2522500034685,-2.35494697412514));
#27986=CARTESIAN_POINT('Ctrl Pts',(-5.30932343282148,62.1252500034686,-4.08005073111967));
#27987=CARTESIAN_POINT('Ctrl Pts',(-6.56268467750003,61.9982500034685,-5.80515448811441));
#27988=CARTESIAN_POINT('Ctrl Pts',(-6.5626846775001,61.8712500034687,-7.93749999999999));
#27989=CARTESIAN_POINT('Ctrl Pts',(-6.56268467750008,61.7442500034686,-10.0698455118856));
#27990=CARTESIAN_POINT('Ctrl Pts',(-5.30932343282148,61.6172500034687,-11.7949492688802));
#27991=CARTESIAN_POINT('Ctrl Pts',(-4.05596218814312,61.4902500034686,-13.5200530258749));
#27992=CARTESIAN_POINT('Ctrl Pts',(-2.0279810940716,61.3632500034687,-14.1789840269267));
#27993=CARTESIAN_POINT('Ctrl Pts',(0.,61.2362500034686,-14.8379150279786));
#27994=CARTESIAN_POINT('Ctrl Pts',(2.0279810940716,61.1092500034687,-14.1789840269267));
#27995=CARTESIAN_POINT('Ctrl Pts',(4.05596218814318,60.9822500034686,-13.5200530258749));
#27996=CARTESIAN_POINT('Ctrl Pts',(5.3093234328217,60.8552500034686,-11.7949492688802));
#27997=CARTESIAN_POINT('Ctrl Pts',(6.56268467750003,60.7282500034687,-10.0698455118856));
#27998=CARTESIAN_POINT('Ctrl Pts',(6.5626846775001,60.6012500034686,-7.93749999999999));
#27999=CARTESIAN_POINT('Ctrl Pts',(6.56268467750008,60.4742500034686,-5.80515448811441));
#28000=CARTESIAN_POINT('Ctrl Pts',(5.30932343282159,60.3472500034687,-4.08005073111967));
#28001=CARTESIAN_POINT('Ctrl Pts',(4.05596218814312,60.2202500034686,-2.35494697412514));
#28002=CARTESIAN_POINT('Ctrl Pts',(2.02798109407165,60.0932500034686,-1.69601597307328));
#28003=CARTESIAN_POINT('Ctrl Pts',(0.,59.9662500034686,-1.0370849720215));
#28004=CARTESIAN_POINT('Ctrl Pts',(-2.02798109407165,59.8392500034686,-1.69601597307317));
#28005=CARTESIAN_POINT('Ctrl Pts',(-4.05596218814306,59.7122500034685,-2.35494697412514));
#28006=CARTESIAN_POINT('Ctrl Pts',(-5.30932343282148,59.5852500034686,-4.08005073111967));
#28007=CARTESIAN_POINT('Ctrl Pts',(-6.56268467750003,59.4582500034686,-5.80515448811441));
#28008=CARTESIAN_POINT('Ctrl Pts',(-6.56268467750004,59.3312500034686,-7.93749999999999));
#28009=CARTESIAN_POINT('Ctrl Pts',(-6.56268467749991,59.2042500034686,-10.0698455118856));
#28010=CARTESIAN_POINT('Ctrl Pts',(-5.30932343282148,59.0772500034686,-11.7949492688802));
#28011=CARTESIAN_POINT('Ctrl Pts',(-4.05596218814312,58.9502500034686,-13.5200530258749));
#28012=CARTESIAN_POINT('Ctrl Pts',(-2.0279810940716,58.8232500034687,-14.1789840269267));
#28013=CARTESIAN_POINT('Ctrl Pts',(0.,58.6962500034686,-14.8379150279786));
#28014=CARTESIAN_POINT('Ctrl Pts',(2.0279810940716,58.5692500034687,-14.1789840269267));
#28015=CARTESIAN_POINT('Ctrl Pts',(4.05596218814318,58.4422500034685,-13.5200530258749));
#28016=CARTESIAN_POINT('Ctrl Pts',(5.30932343282159,58.3152500034686,-11.7949492688802));
#28017=CARTESIAN_POINT('Ctrl Pts',(6.56268467750003,58.1882500034686,-10.0698455118856));
#28018=CARTESIAN_POINT('Ctrl Pts',(6.5626846775001,58.0612500034686,-7.93749999999999));
#28019=CARTESIAN_POINT('Ctrl Pts',(6.56268467749997,57.9342500034686,-5.80515448811441));
#28020=CARTESIAN_POINT('Ctrl Pts',(5.30932343282164,57.8072500034686,-4.08005073111967));
#28021=CARTESIAN_POINT('Ctrl Pts',(4.05596218814318,57.6802500034686,-2.35494697412514));
#28022=CARTESIAN_POINT('Ctrl Pts',(2.02798109407154,57.5532500034686,-1.69601597307317));
#28023=CARTESIAN_POINT('Ctrl Pts',(0.,57.4262500034686,-1.0370849720215));
#28024=CARTESIAN_POINT('Ctrl Pts',(-2.0279810940716,57.2992500034686,-1.69601597307317));
#28025=CARTESIAN_POINT('Ctrl Pts',(-4.05596218814318,57.1722500034686,-2.35494697412514));
#28026=CARTESIAN_POINT('Ctrl Pts',(-5.30932343282148,57.0452500034685,-4.08005073111967));
#28027=CARTESIAN_POINT('Ctrl Pts',(-6.56268467749997,56.9182500034686,-5.80515448811441));
#28028=CARTESIAN_POINT('Ctrl Pts',(-6.56268467750004,56.7912500034686,-7.93749999999999));
#28029=CARTESIAN_POINT('Ctrl Pts',(-6.56268467750003,56.6642500034685,-10.0698455118856));
#28030=CARTESIAN_POINT('Ctrl Pts',(-5.30932343282159,56.5372500034686,-11.7949492688802));
#28031=CARTESIAN_POINT('Ctrl Pts',(-4.05596218814312,56.4102500034685,-13.5200530258749));
#28032=CARTESIAN_POINT('Ctrl Pts',(-2.0279810940716,56.2832500034686,-14.1789840269267));
#28033=CARTESIAN_POINT('Ctrl Pts',(0.,56.1562500034686,-14.8379150279786));
#28034=CARTESIAN_POINT('Ctrl Pts',(2.02798109407165,56.0292500034687,-14.1789840269267));
#28035=CARTESIAN_POINT('Ctrl Pts',(4.05596218814318,55.9022500034686,-13.5200530258749));
#28036=CARTESIAN_POINT('Ctrl Pts',(5.30932343282148,55.7752500034686,-11.7949492688802));
#28037=CARTESIAN_POINT('Ctrl Pts',(6.56268467750003,55.6482500034686,-10.0698455118856));
#28038=CARTESIAN_POINT('Ctrl Pts',(6.5626846775001,55.5212500034686,-7.93749999999999));
#28039=CARTESIAN_POINT('Ctrl Pts',(6.56268467750008,55.3942500034686,-5.80515448811441));
#28040=CARTESIAN_POINT('Ctrl Pts',(5.30932343282153,55.2672500034686,-4.08005073111967));
#28041=CARTESIAN_POINT('Ctrl Pts',(4.05596218814318,55.1402500034686,-2.35494697412514));
#28042=CARTESIAN_POINT('Ctrl Pts',(2.0279810940716,55.0132500034686,-1.69601597307317));
#28043=CARTESIAN_POINT('Ctrl Pts',(-5.83678785436452E-14,54.8862500034686,
-1.0370849720215));
#28044=CARTESIAN_POINT('Ctrl Pts',(-2.0279810940716,54.7592500034686,-1.69601597307323));
#28045=CARTESIAN_POINT('Ctrl Pts',(-4.05596218814318,54.6322500034686,-2.35494697412514));
#28046=CARTESIAN_POINT('Ctrl Pts',(-5.30932343282159,54.5052500034687,-4.08005073111972));
#28047=CARTESIAN_POINT('Ctrl Pts',(-6.56268467749997,54.3782500034686,-5.80515448811441));
#28048=CARTESIAN_POINT('Ctrl Pts',(-6.56268467749999,54.2512500034685,-7.93750000000004));
#28049=CARTESIAN_POINT('Ctrl Pts',(-6.56268467750003,54.1242500034686,-10.0698455118856));
#28050=CARTESIAN_POINT('Ctrl Pts',(-5.30932343282153,53.9972500034686,-11.7949492688803));
#28051=CARTESIAN_POINT('Ctrl Pts',(-4.05596218814318,53.8702500034686,-13.5200530258749));
#28052=CARTESIAN_POINT('Ctrl Pts',(-2.02798109407154,53.7432500034686,-14.1789840269267));
#28053=CARTESIAN_POINT('Ctrl Pts',(0.,53.6162500034685,-14.8379150279786));
#28054=CARTESIAN_POINT('Ctrl Pts',(2.02798109407165,53.4892500034686,-14.1789840269267));
#28055=CARTESIAN_POINT('Ctrl Pts',(4.05596218814312,53.3622500034686,-13.5200530258749));
#28056=CARTESIAN_POINT('Ctrl Pts',(5.30932343282153,53.2352500034686,-11.7949492688803));
#28057=CARTESIAN_POINT('Ctrl Pts',(6.56268467750003,53.1082500034686,-10.0698455118856));
#28058=CARTESIAN_POINT('Ctrl Pts',(6.56268467749999,52.9812500034686,-7.93750000000004));
#28059=CARTESIAN_POINT('Ctrl Pts',(6.56268467749997,52.8542500034685,-5.80515448811441));
#28060=CARTESIAN_POINT('Ctrl Pts',(5.30932343282159,52.7272500034686,-4.08005073111972));
#28061=CARTESIAN_POINT('Ctrl Pts',(4.05596218814318,52.6002500034685,-2.35494697412514));
#28062=CARTESIAN_POINT('Ctrl Pts',(2.0279810940716,52.4732500034685,-1.69601597307323));
#28063=CARTESIAN_POINT('Ctrl Pts',(0.,52.3462500034685,-1.0370849720215));
#28064=CARTESIAN_POINT('Ctrl Pts',(-2.0279810940716,52.2192500034686,-1.69601597307323));
#28065=CARTESIAN_POINT('Ctrl Pts',(-4.05596218814318,52.0922500034686,-2.35494697412514));
#28066=CARTESIAN_POINT('Ctrl Pts',(-5.30932343282153,51.9652500034687,-4.08005073111972));
#28067=CARTESIAN_POINT('Ctrl Pts',(-6.56268467749997,51.8382500034685,-5.80515448811441));
#28068=CARTESIAN_POINT('Ctrl Pts',(-6.56268467749999,51.7112500034686,-7.93750000000004));
#28069=CARTESIAN_POINT('Ctrl Pts',(-6.56268467750003,51.5842500034685,-10.0698455118856));
#28070=CARTESIAN_POINT('Ctrl Pts',(-5.30932343282153,51.4572500034685,-11.7949492688803));
#28071=CARTESIAN_POINT('Ctrl Pts',(-4.05596218814306,51.3302500034686,-13.5200530258749));
#28072=CARTESIAN_POINT('Ctrl Pts',(-2.02798109407154,51.2032500034688,-14.1789840269267));
#28073=CARTESIAN_POINT('Ctrl Pts',(1.1673575708729E-13,51.0762500034686,
-14.8379150279786));
#28074=CARTESIAN_POINT('Ctrl Pts',(2.02798109407154,50.9492500034687,-14.1789840269267));
#28075=CARTESIAN_POINT('Ctrl Pts',(4.05596218814324,50.8222500034686,-13.5200530258749));
#28076=CARTESIAN_POINT('Ctrl Pts',(5.30932343282153,50.6952500034686,-11.7949492688803));
#28077=CARTESIAN_POINT('Ctrl Pts',(6.56268467750003,50.5682500034685,-10.0698455118856));
#28078=CARTESIAN_POINT('Ctrl Pts',(6.56268467749999,50.4412500034686,-7.93750000000004));
#28079=CARTESIAN_POINT('Ctrl Pts',(6.56268467750003,50.3142500034686,-5.80515448811441));
#28080=CARTESIAN_POINT('Ctrl Pts',(5.30932343282159,50.1872500034685,-4.08005073111972));
#28081=CARTESIAN_POINT('Ctrl Pts',(4.05596218814318,50.0602500034686,-2.35494697412514));
#28082=CARTESIAN_POINT('Ctrl Pts',(2.0279810940716,49.9332500034686,-1.69601597307323));
#28083=CARTESIAN_POINT('Ctrl Pts',(1.1673575708729E-13,49.8062500034686,
-1.0370849720215));
#28084=CARTESIAN_POINT('Ctrl Pts',(-2.0279810940716,49.6792500034686,-1.69601597307323));
#28085=CARTESIAN_POINT('Ctrl Pts',(-4.05596218814312,49.5522500034686,-2.35494697412514));
#28086=CARTESIAN_POINT('Ctrl Pts',(-5.30932343282153,49.4252500034686,-4.08005073111972));
#28087=CARTESIAN_POINT('Ctrl Pts',(-6.56268467750008,49.2982500034686,-5.80515448811441));
#28088=CARTESIAN_POINT('Ctrl Pts',(-6.56268467749999,49.1712500034686,-7.93750000000004));
#28089=CARTESIAN_POINT('Ctrl Pts',(-6.56268467750003,49.0442500034686,-10.0698455118856));
#28090=CARTESIAN_POINT('Ctrl Pts',(-5.30932343282148,48.9172500034685,-11.7949492688803));
#28091=CARTESIAN_POINT('Ctrl Pts',(-4.05596218814318,48.7902500034686,-13.5200530258749));
#28092=CARTESIAN_POINT('Ctrl Pts',(-2.02798109407165,48.6632500034687,-14.1789840269267));
#28093=CARTESIAN_POINT('Ctrl Pts',(0.,48.5362500034685,-14.8379150279786));
#28094=CARTESIAN_POINT('Ctrl Pts',(2.0279810940716,48.4092500034688,-14.1789840269267));
#28095=CARTESIAN_POINT('Ctrl Pts',(4.05596218814312,48.2822500034686,-13.5200530258749));
#28096=CARTESIAN_POINT('Ctrl Pts',(5.30932343282159,48.1552500034686,-11.7949492688803));
#28097=CARTESIAN_POINT('Ctrl Pts',(6.56268467750008,48.0282500034685,-10.0698455118856));
#28098=CARTESIAN_POINT('Ctrl Pts',(6.56268467750004,47.9012500034686,-7.93750000000004));
#28099=CARTESIAN_POINT('Ctrl Pts',(6.56268467750003,47.7742500034685,-5.80515448811441));
#28100=CARTESIAN_POINT('Ctrl Pts',(5.30932343282159,47.6472500034686,-4.08005073111972));
#28101=CARTESIAN_POINT('Ctrl Pts',(4.05596218814324,47.5202500034686,-2.35494697412514));
#28102=CARTESIAN_POINT('Ctrl Pts',(2.02798109407165,47.3932500034687,-1.69601597307323));
#28103=CARTESIAN_POINT('Ctrl Pts',(0.,47.2662500034685,-1.0370849720215));
#28104=CARTESIAN_POINT('Ctrl Pts',(-2.02798109407154,47.1392500034686,-1.69601597307323));
#28105=CARTESIAN_POINT('Ctrl Pts',(-4.05596218814312,47.0122500034686,-2.35494697412514));
#28106=CARTESIAN_POINT('Ctrl Pts',(-5.30932343282148,46.8852500034686,-4.08005073111972));
#28107=CARTESIAN_POINT('Ctrl Pts',(-6.56268467749991,46.7582500034686,-5.80515448811441));
#28108=CARTESIAN_POINT('Ctrl Pts',(-6.56268467749999,46.6312500034686,-7.93750000000004));
#28109=CARTESIAN_POINT('Ctrl Pts',(-6.56268467749997,46.5042500034685,-10.0698455118856));
#28110=CARTESIAN_POINT('Ctrl Pts',(-5.30932343282148,46.3772500034686,-11.7949492688803));
#28111=CARTESIAN_POINT('Ctrl Pts',(-4.05596218814312,46.2502500034686,-13.5200530258749));
#28112=CARTESIAN_POINT('Ctrl Pts',(-2.0279810940716,46.1232500034687,-14.1789840269267));
#28113=CARTESIAN_POINT('Ctrl Pts',(0.,45.9962500034685,-14.8379150279786));
#28114=CARTESIAN_POINT('Ctrl Pts',(2.0279810940716,45.8692500034687,-14.1789840269267));
#28115=CARTESIAN_POINT('Ctrl Pts',(4.05596218814312,45.7422500034686,-13.5200530258749));
#28116=CARTESIAN_POINT('Ctrl Pts',(5.30932343282159,45.6152500034686,-11.7949492688803));
#28117=CARTESIAN_POINT('Ctrl Pts',(6.56268467749997,45.4882500034686,-10.0698455118856));
#28118=CARTESIAN_POINT('Ctrl Pts',(6.5626846775001,45.3612500034686,-7.93750000000004));
#28119=CARTESIAN_POINT('Ctrl Pts',(6.56268467750003,45.2342500034686,-5.80515448811441));
#28120=CARTESIAN_POINT('Ctrl Pts',(5.30932343282153,45.1072500034687,-4.08005073111972));
#28121=CARTESIAN_POINT('Ctrl Pts',(4.05596218814312,44.9802500034686,-2.35494697412514));
#28122=CARTESIAN_POINT('Ctrl Pts',(2.02798109407165,44.8532500034686,-1.69601597307323));
#28123=CARTESIAN_POINT('Ctrl Pts',(0.,44.7262500034686,-1.0370849720215));
#28124=CARTESIAN_POINT('Ctrl Pts',(-2.02798109407154,44.5992500034686,-1.69601597307323));
#28125=CARTESIAN_POINT('Ctrl Pts',(-4.05596218814312,44.4722500034685,-2.35494697412514));
#28126=CARTESIAN_POINT('Ctrl Pts',(-5.30932343282148,44.3452500034686,-4.08005073111972));
#28127=CARTESIAN_POINT('Ctrl Pts',(-6.56268467750003,44.2182500034685,-5.80515448811441));
#28128=CARTESIAN_POINT('Ctrl Pts',(-6.56268467750004,44.0912500034686,-7.93750000000004));
#28129=CARTESIAN_POINT('Ctrl Pts',(-6.56268467749997,43.9642500034686,-10.0698455118856));
#28130=CARTESIAN_POINT('Ctrl Pts',(-5.30932343282148,43.8372500034686,-11.7949492688803));
#28131=CARTESIAN_POINT('Ctrl Pts',(-4.05596218814312,43.7102500034686,-13.5200530258749));
#28132=CARTESIAN_POINT('Ctrl Pts',(-2.0279810940716,43.5832500034687,-14.1789840269267));
#28133=CARTESIAN_POINT('Ctrl Pts',(0.,43.4562500034686,-14.8379150279786));
#28134=CARTESIAN_POINT('Ctrl Pts',(2.0279810940716,43.3292500034687,-14.1789840269267));
#28135=CARTESIAN_POINT('Ctrl Pts',(4.05596218814312,43.2022500034685,-13.5200530258749));
#28136=CARTESIAN_POINT('Ctrl Pts',(5.30932343282159,43.0752500034686,-11.7949492688803));
#28137=CARTESIAN_POINT('Ctrl Pts',(6.56268467750008,42.9482500034686,-10.0698455118856));
#28138=CARTESIAN_POINT('Ctrl Pts',(6.5626846775001,42.8212500034686,-7.93750000000004));
#28139=CARTESIAN_POINT('Ctrl Pts',(6.56268467750003,42.6942500034686,-5.80515448811441));
#28140=CARTESIAN_POINT('Ctrl Pts',(5.30932343282153,42.5672500034686,-4.08005073111972));
#28141=CARTESIAN_POINT('Ctrl Pts',(4.05596218814324,42.4402500034686,-2.35494697412514));
#28142=CARTESIAN_POINT('Ctrl Pts',(2.02798109407165,42.3132500034686,-1.69601597307323));
#28143=CARTESIAN_POINT('Ctrl Pts',(0.,42.1862500034686,-1.0370849720215));
#28144=CARTESIAN_POINT('Ctrl Pts',(-2.0279810940716,42.0592500034685,-1.69601597307323));
#28145=CARTESIAN_POINT('Ctrl Pts',(-4.05596218814312,41.9322500034686,-2.35494697412514));
#28146=CARTESIAN_POINT('Ctrl Pts',(-5.30932343282148,41.8052500034685,-4.08005073111972));
#28147=CARTESIAN_POINT('Ctrl Pts',(-6.56268467750003,41.6782500034686,-5.80515448811441));
#28148=CARTESIAN_POINT('Ctrl Pts',(-6.56268467750004,41.5512500034686,-7.93750000000004));
#28149=CARTESIAN_POINT('Ctrl Pts',(-6.56268467749997,41.4242500034686,-10.0698455118856));
#28150=CARTESIAN_POINT('Ctrl Pts',(-5.30932343282153,41.2972500034686,-11.7949492688803));
#28151=CARTESIAN_POINT('Ctrl Pts',(-4.05596218814312,41.1702500034685,-13.5200530258749));
#28152=CARTESIAN_POINT('Ctrl Pts',(-2.0279810940716,41.0432500034686,-14.1789840269267));
#28153=CARTESIAN_POINT('Ctrl Pts',(0.,40.9162500034686,-14.8379150279786));
#28154=CARTESIAN_POINT('Ctrl Pts',(2.02798109407165,40.7892500034687,-14.1789840269267));
#28155=CARTESIAN_POINT('Ctrl Pts',(4.05596218814312,40.6622500034685,-13.5200530258749));
#28156=CARTESIAN_POINT('Ctrl Pts',(5.30932343282153,40.5352500034686,-11.7949492688803));
#28157=CARTESIAN_POINT('Ctrl Pts',(6.56268467749997,40.4082500034686,-10.0698455118856));
#28158=CARTESIAN_POINT('Ctrl Pts',(6.5626846775001,40.2812500034686,-7.93750000000004));
#28159=CARTESIAN_POINT('Ctrl Pts',(6.56268467750008,40.1542500034685,-5.80515448811441));
#28160=CARTESIAN_POINT('Ctrl Pts',(5.30932343282153,40.0272500034686,-4.08005073111972));
#28161=CARTESIAN_POINT('Ctrl Pts',(4.05596218814312,39.9002500034686,-2.35494697412514));
#28162=CARTESIAN_POINT('Ctrl Pts',(2.0279810940716,39.7732500034685,-1.69601597307323));
#28163=CARTESIAN_POINT('Ctrl Pts',(0.,39.6462500034686,-1.0370849720215));
#28164=CARTESIAN_POINT('Ctrl Pts',(-2.0279810940716,39.5192500034686,-1.69601597307323));
#28165=CARTESIAN_POINT('Ctrl Pts',(-4.05596218814324,39.3922500034686,-2.35494697412514));
#28166=CARTESIAN_POINT('Ctrl Pts',(-5.30932343282148,39.2652500034686,-4.08005073111972));
#28167=CARTESIAN_POINT('Ctrl Pts',(-6.56268467749991,39.1382500034686,-5.80515448811441));
#28168=CARTESIAN_POINT('Ctrl Pts',(-6.56268467749999,39.0112500034685,-7.93750000000004));
#28169=CARTESIAN_POINT('Ctrl Pts',(-6.56268467750008,38.8842500034686,-10.0698455118856));
#28170=CARTESIAN_POINT('Ctrl Pts',(-5.30932343282153,38.7572500034686,-11.7949492688803));
#28171=CARTESIAN_POINT('Ctrl Pts',(-4.05596218814312,38.6302500034686,-13.5200530258749));
#28172=CARTESIAN_POINT('Ctrl Pts',(-2.02798109407154,38.5032500034686,-14.1789840269267));
#28173=CARTESIAN_POINT('Ctrl Pts',(0.,38.3762500034685,-14.8379150279786));
#28174=CARTESIAN_POINT('Ctrl Pts',(2.02798109407165,38.2492500034686,-14.1789840269267));
#28175=CARTESIAN_POINT('Ctrl Pts',(4.05596218814318,38.1222500034686,-13.5200530258749));
#28176=CARTESIAN_POINT('Ctrl Pts',(5.30932343282153,37.9952500034686,-11.7949492688803));
#28177=CARTESIAN_POINT('Ctrl Pts',(6.56268467750003,37.8682500034686,-10.0698455118856));
#28178=CARTESIAN_POINT('Ctrl Pts',(6.56268467749999,37.7412500034686,-7.93750000000004));
#28179=CARTESIAN_POINT('Ctrl Pts',(6.56268467750008,37.6142500034686,-5.80515448811441));
#28180=CARTESIAN_POINT('Ctrl Pts',(5.30932343282159,37.4872500034686,-4.08005073111972));
#28181=CARTESIAN_POINT('Ctrl Pts',(4.05596218814312,37.3602500034685,-2.35494697412514));
#28182=CARTESIAN_POINT('Ctrl Pts',(2.0279810940716,37.2332500034685,-1.69601597307323));
#28183=CARTESIAN_POINT('Ctrl Pts',(-1.1673575708729E-13,37.1062500034685,
-1.0370849720215));
#28184=CARTESIAN_POINT('Ctrl Pts',(-2.0279810940716,36.9792500034686,-1.69601597307323));
#28185=CARTESIAN_POINT('Ctrl Pts',(-4.05596218814306,36.8522500034687,-2.35494697412514));
#28186=CARTESIAN_POINT('Ctrl Pts',(-5.30932343282153,36.7252500034687,-4.08005073111972));
#28187=CARTESIAN_POINT('Ctrl Pts',(-6.56268467750003,36.5982500034685,-5.80515448811441));
#28188=CARTESIAN_POINT('Ctrl Pts',(-6.56268467749999,36.4712500034686,-7.93750000000004));
#28189=CARTESIAN_POINT('Ctrl Pts',(-6.56268467749991,36.3442500034685,-10.0698455118856));
#28190=CARTESIAN_POINT('Ctrl Pts',(-5.30932343282153,36.2172500034686,-11.7949492688803));
#28191=CARTESIAN_POINT('Ctrl Pts',(-4.05596218814312,36.0902500034685,-13.5200530258749));
#28192=CARTESIAN_POINT('Ctrl Pts',(-2.02798109407154,35.9632500034688,-14.1789840269267));
#28193=CARTESIAN_POINT('Ctrl Pts',(0.,35.8362500034686,-14.8379150279786));
#28194=CARTESIAN_POINT('Ctrl Pts',(2.02798109407165,35.7092500034686,-14.1789840269267));
#28195=CARTESIAN_POINT('Ctrl Pts',(4.05596218814318,35.5822500034686,-13.5200530258749));
#28196=CARTESIAN_POINT('Ctrl Pts',(5.30932343282153,35.4552500034687,-11.7949492688803));
#28197=CARTESIAN_POINT('Ctrl Pts',(6.56268467750003,35.3282500034686,-10.0698455118856));
#28198=CARTESIAN_POINT('Ctrl Pts',(6.56268467749999,35.2012500034686,-7.93750000000004));
#28199=CARTESIAN_POINT('Ctrl Pts',(6.56268467749997,35.0742500034685,-5.80515448811441));
#28200=CARTESIAN_POINT('Ctrl Pts',(5.30932343282159,34.9472500034685,-4.08005073111972));
#28201=CARTESIAN_POINT('Ctrl Pts',(4.05596218814318,34.8202500034686,-2.35494697412514));
#28202=CARTESIAN_POINT('Ctrl Pts',(2.0279810940716,34.6932500034686,-1.69601597307323));
#28203=CARTESIAN_POINT('Ctrl Pts',(0.,34.5662500034686,-1.0370849720215));
#28204=CARTESIAN_POINT('Ctrl Pts',(-2.0279810940716,34.4392500034686,-1.69601597307323));
#28205=CARTESIAN_POINT('Ctrl Pts',(-4.05596218814318,34.3122500034686,-2.35494697412514));
#28206=CARTESIAN_POINT('Ctrl Pts',(-5.30932343282153,34.1852500034686,-4.08005073111972));
#28207=CARTESIAN_POINT('Ctrl Pts',(-6.56268467749997,34.0582500034686,-5.80515448811441));
#28208=CARTESIAN_POINT('Ctrl Pts',(-6.56268467749999,33.9312500034686,-7.93750000000004));
#28209=CARTESIAN_POINT('Ctrl Pts',(-6.56268467750003,33.8042500034686,-10.0698455118856));
#28210=CARTESIAN_POINT('Ctrl Pts',(-5.30932343282148,33.6772500034685,-11.7949492688803));
#28211=CARTESIAN_POINT('Ctrl Pts',(-4.05596218814306,33.5502500034685,-13.5200530258749));
#28212=CARTESIAN_POINT('Ctrl Pts',(-2.02798109407154,33.4232500034688,-14.1789840269267));
#28213=CARTESIAN_POINT('Ctrl Pts',(0.,33.2962500034685,-14.8379150279786));
#28214=CARTESIAN_POINT('Ctrl Pts',(2.02798109407165,33.1692500034688,-14.1789840269267));
#28215=CARTESIAN_POINT('Ctrl Pts',(4.05596218814318,33.0422500034686,-13.5200530258749));
#28216=CARTESIAN_POINT('Ctrl Pts',(5.30932343282159,32.9152500034686,-11.7949492688803));
#28217=CARTESIAN_POINT('Ctrl Pts',(6.56268467750003,32.7882500034685,-10.0698455118856));
#28218=CARTESIAN_POINT('Ctrl Pts',(6.56268467750004,32.6612500034686,-7.93750000000004));
#28219=CARTESIAN_POINT('Ctrl Pts',(6.56268467750008,32.5342500034685,-5.80515448811441));
#28220=CARTESIAN_POINT('Ctrl Pts',(5.30932343282159,32.4072500034686,-4.08005073111972));
#28221=CARTESIAN_POINT('Ctrl Pts',(4.05596218814318,32.2802500034685,-2.35494697412514));
#28222=CARTESIAN_POINT('Ctrl Pts',(2.02798109407165,32.1532500034687,-1.69601597307323));
#28223=CARTESIAN_POINT('Ctrl Pts',(0.,32.0262500034685,-1.0370849720215));
#28224=CARTESIAN_POINT('Ctrl Pts',(-2.02798109407154,31.8992500034685,-1.69601597307323));
#28225=CARTESIAN_POINT('Ctrl Pts',(-4.05596218814318,31.7722500034685,-2.35494697412514));
#28226=CARTESIAN_POINT('Ctrl Pts',(-5.30932343282148,31.6452500034686,-4.08005073111972));
#28227=CARTESIAN_POINT('Ctrl Pts',(-6.56268467749997,31.5182500034685,-5.80515448811441));
#28228=CARTESIAN_POINT('Ctrl Pts',(-6.56268467749999,31.3912500034687,-7.93750000000004));
#28229=CARTESIAN_POINT('Ctrl Pts',(-6.56268467750003,31.2642500034685,-10.0698455118856));
#28230=CARTESIAN_POINT('Ctrl Pts',(-5.30932343282148,31.1372500034686,-11.7949492688803));
#28231=CARTESIAN_POINT('Ctrl Pts',(-4.05596218814318,31.0102500034686,-13.5200530258749));
#28232=CARTESIAN_POINT('Ctrl Pts',(-2.0279810940716,30.8832500034687,-14.1789840269267));
#28233=CARTESIAN_POINT('Ctrl Pts',(0.,30.7562500034685,-14.8379150279786));
#28234=CARTESIAN_POINT('Ctrl Pts',(2.0279810940716,30.6292500034687,-14.1789840269267));
#28235=CARTESIAN_POINT('Ctrl Pts',(4.05596218814312,30.5022500034686,-13.5200530258749));
#28236=CARTESIAN_POINT('Ctrl Pts',(5.30932343282159,30.3752500034686,-11.7949492688803));
#28237=CARTESIAN_POINT('Ctrl Pts',(6.56268467750003,30.2482500034686,-10.0698455118856));
#28238=CARTESIAN_POINT('Ctrl Pts',(6.5626846775001,30.1212500034686,-7.93750000000004));
#28239=CARTESIAN_POINT('Ctrl Pts',(6.56268467750003,29.9942500034686,-5.80515448811441));
#28240=CARTESIAN_POINT('Ctrl Pts',(5.30932343282159,29.8672500034686,-4.08005073111972));
#28241=CARTESIAN_POINT('Ctrl Pts',(4.05596218814318,29.7402500034686,-2.35494697412514));
#28242=CARTESIAN_POINT('Ctrl Pts',(2.02798109407165,29.6132500034686,-1.69601597307323));
#28243=CARTESIAN_POINT('Ctrl Pts',(0.,29.4862500034686,-1.0370849720215));
#28244=CARTESIAN_POINT('Ctrl Pts',(-2.02798109407154,29.3592500034686,-1.69601597307323));
#28245=CARTESIAN_POINT('Ctrl Pts',(-4.05596218814312,29.2322500034686,-2.35494697412503));
#28246=CARTESIAN_POINT('Ctrl Pts',(-5.30932343282159,29.1052500034686,-4.08005073111972));
#28247=CARTESIAN_POINT('Ctrl Pts',(-6.56268467749997,28.9782500034685,-5.80515448811441));
#28248=CARTESIAN_POINT('Ctrl Pts',(-6.56268467749993,28.8512500034686,-7.93750000000004));
#28249=CARTESIAN_POINT('Ctrl Pts',(-6.56268467750003,28.7242500034685,-10.0698455118856));
#28250=CARTESIAN_POINT('Ctrl Pts',(-5.30932343282159,28.5972500034687,-11.7949492688803));
#28251=CARTESIAN_POINT('Ctrl Pts',(-4.05596218814306,28.4702500034686,-13.5200530258749));
#28252=CARTESIAN_POINT('Ctrl Pts',(-2.0279810940716,28.3432500034687,-14.1789840269267));
#28253=CARTESIAN_POINT('Ctrl Pts',(1.1673575708729E-13,28.2162500034685,
-14.8379150279786));
#28254=CARTESIAN_POINT('Ctrl Pts',(2.0279810940716,28.0892500034687,-14.1789840269267));
#28255=CARTESIAN_POINT('Ctrl Pts',(4.05596218814324,27.9622500034685,-13.5200530258749));
#28256=CARTESIAN_POINT('Ctrl Pts',(5.30932343282159,27.8352500034685,-11.7949492688803));
#28257=CARTESIAN_POINT('Ctrl Pts',(6.56268467750003,27.7082500034685,-10.0698455118856));
#28258=CARTESIAN_POINT('Ctrl Pts',(6.5626846775001,27.5812500034686,-7.93750000000004));
#28259=CARTESIAN_POINT('Ctrl Pts',(6.56268467750003,27.4542500034686,-5.80515448811441));
#28260=CARTESIAN_POINT('Ctrl Pts',(5.30932343282153,27.3272500034686,-4.08005073111972));
#28261=CARTESIAN_POINT('Ctrl Pts',(4.05596218814312,27.2002500034686,-2.35494697412514));
#28262=CARTESIAN_POINT('Ctrl Pts',(2.02798109407165,27.0732500034686,-1.69601597307323));
#28263=CARTESIAN_POINT('Ctrl Pts',(1.1673575708729E-13,26.9462500034685,
-1.0370849720215));
#28264=CARTESIAN_POINT('Ctrl Pts',(-2.02798109407148,26.8192500034686,-1.69601597307323));
#28265=CARTESIAN_POINT('Ctrl Pts',(-4.05596218814312,26.6922500034685,-2.35494697412503));
#28266=CARTESIAN_POINT('Ctrl Pts',(-5.30932343282159,26.5652500034685,-4.08005073111972));
#28267=CARTESIAN_POINT('Ctrl Pts',(-6.56268467750008,26.4382500034685,-5.80515448811441));
#28268=CARTESIAN_POINT('Ctrl Pts',(-6.56268467750004,26.3112500034686,-7.93750000000004));
#28269=CARTESIAN_POINT('Ctrl Pts',(-6.56268467749997,26.1842500034686,-10.0698455118856));
#28270=CARTESIAN_POINT('Ctrl Pts',(-5.30932343282159,26.0572500034686,-11.7949492688803));
#28271=CARTESIAN_POINT('Ctrl Pts',(-4.05596218814318,25.9302500034685,-13.5200530258749));
#28272=CARTESIAN_POINT('Ctrl Pts',(-2.0279810940716,25.8032500034687,-14.1789840269267));
#28273=CARTESIAN_POINT('Ctrl Pts',(0.,25.6762500034686,-14.8379150279786));
#28274=CARTESIAN_POINT('Ctrl Pts',(2.02798109407165,25.5492500034687,-14.1789840269267));
#28275=CARTESIAN_POINT('Ctrl Pts',(4.05596218814312,25.4222500034686,-13.5200530258749));
#28276=CARTESIAN_POINT('Ctrl Pts',(5.30932343282153,25.2952500034686,-11.7949492688803));
#28277=CARTESIAN_POINT('Ctrl Pts',(6.56268467750008,25.1682500034686,-10.0698455118856));
#28278=CARTESIAN_POINT('Ctrl Pts',(6.5626846775001,25.0412500034685,-7.93750000000004));
#28279=CARTESIAN_POINT('Ctrl Pts',(6.56268467750003,24.9142500034686,-5.80515448811441));
#28280=CARTESIAN_POINT('Ctrl Pts',(5.30932343282153,24.7872500034686,-4.08005073111972));
#28281=CARTESIAN_POINT('Ctrl Pts',(4.05596218814324,24.6602500034686,-2.35494697412514));
#28282=CARTESIAN_POINT('Ctrl Pts',(2.02798109407171,24.5332500034686,-1.69601597307323));
#28283=CARTESIAN_POINT('Ctrl Pts',(0.,24.4062500034686,-1.0370849720215));
#28284=CARTESIAN_POINT('Ctrl Pts',(-2.0279810940716,24.2792500034685,-1.69601597307323));
#28285=CARTESIAN_POINT('Ctrl Pts',(-4.05596218814312,24.1522500034685,-2.35494697412503));
#28286=CARTESIAN_POINT('Ctrl Pts',(-5.30932343282159,24.0252500034685,-4.08005073111972));
#28287=CARTESIAN_POINT('Ctrl Pts',(-6.56268467749991,23.8982500034686,-5.80515448811441));
#28288=CARTESIAN_POINT('Ctrl Pts',(-6.56268467749999,23.7712500034686,-7.93750000000004));
#28289=CARTESIAN_POINT('Ctrl Pts',(-6.56268467749997,23.6442500034686,-10.0698455118856));
#28290=CARTESIAN_POINT('Ctrl Pts',(-5.30932343282164,23.5172500034686,-11.7949492688803));
#28291=CARTESIAN_POINT('Ctrl Pts',(-4.05596218814312,23.3902500034686,-13.5200530258749));
#28292=CARTESIAN_POINT('Ctrl Pts',(-2.02798109407154,23.2632500034686,-14.1789840269267));
#28293=CARTESIAN_POINT('Ctrl Pts',(0.,23.1362500034685,-14.8379150279786));
#28294=CARTESIAN_POINT('Ctrl Pts',(2.02798109407165,23.0092500034686,-14.1789840269267));
#28295=CARTESIAN_POINT('Ctrl Pts',(4.05596218814312,22.8822500034685,-13.5200530258749));
#28296=CARTESIAN_POINT('Ctrl Pts',(5.30932343282153,22.7552500034686,-11.7949492688803));
#28297=CARTESIAN_POINT('Ctrl Pts',(6.56268467749997,22.6282500034686,-10.0698455118856));
#28298=CARTESIAN_POINT('Ctrl Pts',(6.5626846775001,22.5012500034686,-7.93750000000004));
#28299=CARTESIAN_POINT('Ctrl Pts',(6.56268467750003,22.3742500034686,-5.80515448811441));
#28300=CARTESIAN_POINT('Ctrl Pts',(5.30932343282159,22.2472500034686,-4.08005073111972));
#28301=CARTESIAN_POINT('Ctrl Pts',(4.05596218814312,22.1202500034686,-2.35494697412503));
#28302=CARTESIAN_POINT('Ctrl Pts',(2.0279810940716,21.9932500034685,-1.69601597307323));
#28303=CARTESIAN_POINT('Ctrl Pts',(0.,21.8662500034686,-1.0370849720215));
#28304=CARTESIAN_POINT('Ctrl Pts',(-2.0279810940716,21.7392500034686,-1.69601597307323));
#28305=CARTESIAN_POINT('Ctrl Pts',(-4.05596218814312,21.6122500034686,-2.35494697412503));
#28306=CARTESIAN_POINT('Ctrl Pts',(-5.30932343282153,21.4852500034687,-4.08005073111972));
#28307=CARTESIAN_POINT('Ctrl Pts',(-6.56268467750003,21.3582500034686,-5.80515448811441));
#28308=CARTESIAN_POINT('Ctrl Pts',(-6.56268467749999,21.2312500034685,-7.93750000000004));
#28309=CARTESIAN_POINT('Ctrl Pts',(-6.56268467749997,21.1042500034685,-10.0698455118856));
#28310=CARTESIAN_POINT('Ctrl Pts',(-5.30932343282164,20.9772500034686,-11.7949492688803));
#28311=CARTESIAN_POINT('Ctrl Pts',(-4.05596218814312,20.8502500034685,-13.5200530258749));
#28312=CARTESIAN_POINT('Ctrl Pts',(-2.02798109407154,20.7232500034687,-14.1789840269267));
#28313=CARTESIAN_POINT('Ctrl Pts',(0.,20.5962500034686,-14.8379150279786));
#28314=CARTESIAN_POINT('Ctrl Pts',(2.02798109407171,20.4692500034686,-14.1789840269267));
#28315=CARTESIAN_POINT('Ctrl Pts',(4.05596218814324,20.3422500034686,-13.5200530258749));
#28316=CARTESIAN_POINT('Ctrl Pts',(5.30932343282159,20.2152500034686,-11.7949492688803));
#28317=CARTESIAN_POINT('Ctrl Pts',(6.56268467750008,20.0882500034685,-10.0698455118856));
#28318=CARTESIAN_POINT('Ctrl Pts',(6.56268467749999,19.9612500034686,-7.93750000000004));
#28319=CARTESIAN_POINT('Ctrl Pts',(6.56268467750003,19.8342500034686,-5.80515448811441));
#28320=CARTESIAN_POINT('Ctrl Pts',(5.30932343282159,19.7072500034685,-4.08005073111972));
#28321=CARTESIAN_POINT('Ctrl Pts',(4.65426850829619,19.6408749054927,-3.17844497608727));
#28322=CARTESIAN_POINT('Ctrl Pts',(3.73830419723802,19.5711012915162,-2.54362273914156));
#28323=CARTESIAN_POINT('Ctrl Pts',(-4.37003557241966,17.7638095496546,-15.102482089171));
#28324=CARTESIAN_POINT('Ctrl Pts',(-4.2103702834995,18.1928079871481,-14.6678643719681));
#28325=CARTESIAN_POINT('Ctrl Pts',(-4.33444454882375,18.8064629622641,-14.587046595076));
#28326=CARTESIAN_POINT('Ctrl Pts',(-4.08157677823063,17.9187863946121,-15.1900626743679));
#28327=CARTESIAN_POINT('Ctrl Pts',(-3.94432134458797,18.3471485010018,-14.8326958966496));
#28328=CARTESIAN_POINT('Ctrl Pts',(-4.00038492834513,18.920735573139,-14.8048348003922));
#28329=CARTESIAN_POINT('Ctrl Pts',(-3.75474604664856,18.0355130533343,-15.2941158606652));
#28330=CARTESIAN_POINT('Ctrl Pts',(-3.63142428276688,18.4451150135817,-15.0057172827804));
#28331=CARTESIAN_POINT('Ctrl Pts',(-3.64549788804367,18.9604219221267,-14.9998486582339));
#28332=CARTESIAN_POINT('Ctrl Pts',(-3.06702447279691,18.1853704931012,-15.4855412059039));
#28333=CARTESIAN_POINT('Ctrl Pts',(-2.96645051654635,18.5378312167901,-15.3082202157406));
#28334=CARTESIAN_POINT('Ctrl Pts',(-2.92607963880819,18.943217221379,-15.3261118803759));
#28335=CARTESIAN_POINT('Ctrl Pts',(-2.70267020745179,18.2245844759334,-15.5753399203331));
#28336=CARTESIAN_POINT('Ctrl Pts',(-2.61131057061418,18.5396307567559,-15.442931788489));
#28337=CARTESIAN_POINT('Ctrl Pts',(-2.55821925230425,18.8884651665,-15.4610221924584));
#28338=CARTESIAN_POINT('Ctrl Pts',(-1.96287492552905,18.2420368665519,-15.7200549564683));
#28339=CARTESIAN_POINT('Ctrl Pts',(-1.89153946623817,18.4751290933259,-15.6554598329745));
#28340=CARTESIAN_POINT('Ctrl Pts',(-1.82891453529875,18.7188972454106,-15.6707363824264));
#28341=CARTESIAN_POINT('Ctrl Pts',(-1.58083481983854,18.222769633288,-15.7776716447618));
#28342=CARTESIAN_POINT('Ctrl Pts',(-1.52010391061206,18.4109075711029,-15.7376927898266));
#28343=CARTESIAN_POINT('Ctrl Pts',(-1.46353132936861,18.6039976265509,-15.7477141627275));
#28344=CARTESIAN_POINT('Ctrl Pts',(-0.800159047972911,18.1403974723434,
-15.8549367200197));
#28345=CARTESIAN_POINT('Ctrl Pts',(-0.765887806043689,18.2357094897268,
-15.8471046363309));
#28346=CARTESIAN_POINT('Ctrl Pts',(-0.72911749444839,18.3301937694425,-15.8501327855033));
#28347=CARTESIAN_POINT('Ctrl Pts',(-0.3987363866075,18.0770350176174,-15.8749999999984));
#28348=CARTESIAN_POINT('Ctrl Pts',(-0.379968212271851,18.1240305159854,
-15.8749999999992));
#28349=CARTESIAN_POINT('Ctrl Pts',(-0.361264584887649,18.1710404017991,
-15.875));
#28350=CARTESIAN_POINT('Ctrl Pts',(4.96157977224833E-14,18.0000000000001,
-15.875));
#28351=CARTESIAN_POINT('Ctrl Pts',(4.96157977224833E-14,18.0000000000001,
-15.875));
#28352=CARTESIAN_POINT('Ctrl Pts',(4.96157977224833E-14,18.0000000000001,
-15.875));
#28353=CARTESIAN_POINT('',(-4.26261338778688,18.0849267018157,-14.875));
#28354=CARTESIAN_POINT('Ctrl Pts',(5.55111512312578E-14,18.0000000000001,
-15.875));
#28355=CARTESIAN_POINT('Ctrl Pts',(-0.733684917776591,18.1419056781966,
-15.875));
#28356=CARTESIAN_POINT('Ctrl Pts',(-1.47554802668037,18.248989994314,-15.8100424832836));
#28357=CARTESIAN_POINT('Ctrl Pts',(-2.37917217060925,18.2923856158391,-15.6165480209598));
#28358=CARTESIAN_POINT('Ctrl Pts',(-2.55900832274013,18.2964779051254,-15.5720852748806));
#28359=CARTESIAN_POINT('Ctrl Pts',(-2.91667689706805,18.2933500475869,-15.4698863303733));
#28360=CARTESIAN_POINT('Ctrl Pts',(-3.09551309904666,18.2860499025369,-15.4117537005875));
#28361=CARTESIAN_POINT('Ctrl Pts',(-3.61925135711828,18.2429598209237,-15.2173122956099));
#28362=CARTESIAN_POINT('Ctrl Pts',(-3.95179505566483,18.1882637114374,-15.0609272799604));
#28363=CARTESIAN_POINT('Ctrl Pts',(-4.26261338778688,18.0849267018157,-14.875));
#28364=CARTESIAN_POINT('Origin',(-5.10514446416555,18.819869818891,-15.875));
#28365=CARTESIAN_POINT('Ctrl Pts',(-4.29373077449685,18.819869818891,-14.6134105960265));
#28366=CARTESIAN_POINT('Ctrl Pts',(-4.05040020405459,17.5517750653647,-14.7699129852744));
#28367=CARTESIAN_POINT('Ctrl Pts',(-4.71244104384512,17.3721875251302,-15.875));
#28368=CARTESIAN_POINT('Ctrl Pts',(-4.85172205446064,18.6399031555503,-14.254528568441));
#28369=CARTESIAN_POINT('Ctrl Pts',(-4.60179941715923,17.4268547635552,-14.4435616230053));
#28370=CARTESIAN_POINT('Ctrl Pts',(-5.32488118024252,17.2060548471653,-15.4482730708507));
#28371=CARTESIAN_POINT('Ctrl Pts',(-5.35047866129627,18.4418014142638,-13.8366896334367));
#28372=CARTESIAN_POINT('Ctrl Pts',(-5.12064004592465,17.2814545873273,-14.047160515657));
#28373=CARTESIAN_POINT('Ctrl Pts',(-5.872239451894,17.0232013062602,-14.9514971234146));
#28374=CARTESIAN_POINT('Ctrl Pts',(-6.01799603717833,18.142003732685,-13.1234105702918));
#28375=CARTESIAN_POINT('Ctrl Pts',(-5.8322275983879,17.0508424851127,-13.3390649200856));
#28376=CARTESIAN_POINT('Ctrl Pts',(-6.60485088974141,16.746464983624,-14.1034251661552));
#28377=CARTESIAN_POINT('Ctrl Pts',(-6.22802018553564,18.0410299920571,-12.8694063525054));
#28378=CARTESIAN_POINT('Ctrl Pts',(-6.05721596844286,16.9724647253111,-13.085858679893));
#28379=CARTESIAN_POINT('Ctrl Pts',(-6.83535589111353,16.6532584546768,-13.8014201512646));
#28380=CARTESIAN_POINT('Ctrl Pts',(-6.6144435597649,17.845539227244,-12.3376218274051));
#28381=CARTESIAN_POINT('Ctrl Pts',(-6.47397956801525,16.8187344562347,-12.5492603262157));
#28382=CARTESIAN_POINT('Ctrl Pts',(-7.25946198077295,16.4728054400627,-13.1691409130384));
#28383=CARTESIAN_POINT('Ctrl Pts',(-6.78984519594626,17.7516276808024,-12.0616732803204));
#28384=CARTESIAN_POINT('Ctrl Pts',(-6.66536331485427,16.7437399954129,-12.2678113800685));
#28385=CARTESIAN_POINT('Ctrl Pts',(-7.45196819832983,16.3861178595998,-12.841044608914));
#28386=CARTESIAN_POINT('Ctrl Pts',(-7.1060232070069,17.5758144266797,-11.4892935205334));
#28387=CARTESIAN_POINT('Ctrl Pts',(-7.01161694949603,16.6021903559506,-11.6791754308633));
#28388=CARTESIAN_POINT('Ctrl Pts',(-7.79897883144068,16.2238287011529,-12.1604985952507));
#28389=CARTESIAN_POINT('Ctrl Pts',(-7.24680107601186,17.4939013437499,-11.1928654121415));
#28390=CARTESIAN_POINT('Ctrl Pts',(-7.1672942491468,16.53538393131,-11.3716926957734));
#28391=CARTESIAN_POINT('Ctrl Pts',(-7.95348488826811,16.1482166253278,-11.8080525767787));
#28392=CARTESIAN_POINT('Ctrl Pts',(-7.49273513776195,17.3468185637659,-10.5780397094536));
#28393=CARTESIAN_POINT('Ctrl Pts',(-7.43969881407854,16.4148594991967,-10.7303703061362));
#28394=CARTESIAN_POINT('Ctrl Pts',(-8.22340161649152,16.0124479046868,-11.0770393394486));
#28395=CARTESIAN_POINT('Ctrl Pts',(-7.59843488959469,17.2812951267938,-10.2569047180054));
#28396=CARTESIAN_POINT('Ctrl Pts',(-7.55776347710441,16.3605717978341,-10.393033282372));
#28397=CARTESIAN_POINT('Ctrl Pts',(-8.33940885518503,15.9519647326955,-10.6952174205744));
#28398=CARTESIAN_POINT('Ctrl Pts',(-7.85078664959267,17.1222147255269,-9.28539995987796));
#28399=CARTESIAN_POINT('Ctrl Pts',(-7.83853818369,16.229043980975,-9.37303471985337));
#28400=CARTESIAN_POINT('Ctrl Pts',(-8.6163691151618,15.8051212845607,-9.5401212122307));
#28401=CARTESIAN_POINT('Ctrl Pts',(-7.93672823551223,17.0646099827074,-8.62351488694819));
#28402=CARTESIAN_POINT('Ctrl Pts',(-7.93663307907031,16.1799952820739,-8.6658176185236));
#28403=CARTESIAN_POINT('Ctrl Pts',(-8.71069143789301,15.751947676348,-8.75315549550617));
#28404=CARTESIAN_POINT('Ctrl Pts',(-7.93768657939644,17.0639797987105,-7.77723195581193));
#28405=CARTESIAN_POINT('Ctrl Pts',(-7.93770957586298,16.1794674107193,-7.76735582075032));
#28406=CARTESIAN_POINT('Ctrl Pts',(-8.71174323535012,15.7513659680398,-7.74694508131947));
#28407=CARTESIAN_POINT('Ctrl Pts',(-7.93240014505282,17.0674607979061,-7.60633724591963));
#28408=CARTESIAN_POINT('Ctrl Pts',(-7.93176509524179,16.1823866550743,-7.58584716868171));
#28409=CARTESIAN_POINT('Ctrl Pts',(-8.70594128558497,15.7545791980315,-7.54375530815316));
#28410=CARTESIAN_POINT('Ctrl Pts',(-7.91102975013305,17.0814770208683,-7.2679859049775));
#28411=CARTESIAN_POINT('Ctrl Pts',(-7.90776940619295,16.1941201670182,-7.22681048952224));
#28412=CARTESIAN_POINT('Ctrl Pts',(-8.68248692160874,15.767517250068,-7.14146355629932));
#28413=CARTESIAN_POINT('Ctrl Pts',(-7.89499158493917,17.0919817317593,-7.10010500886008));
#28414=CARTESIAN_POINT('Ctrl Pts',(-7.88974897820912,16.2029188357821,-7.04867703153029));
#28415=CARTESIAN_POINT('Ctrl Pts',(-8.66488476781423,15.7772139061693,-6.94185713653414));
#28416=CARTESIAN_POINT('Ctrl Pts',(-7.831248853586,17.1334594467781,-6.60022193131186));
#28417=CARTESIAN_POINT('Ctrl Pts',(-7.81819429110638,16.2376097544146,-6.51852828695844));
#28418=CARTESIAN_POINT('Ctrl Pts',(-8.59492605887025,15.8155010279353,-6.34750796554458));
#28419=CARTESIAN_POINT('Ctrl Pts',(-7.76798084410886,17.1743995785599,-6.27196753629823));
#28420=CARTESIAN_POINT('Ctrl Pts',(-7.74705485466677,16.2718853507128,-6.17083955222712));
#28421=CARTESIAN_POINT('Ctrl Pts',(-8.5254883642425,15.8532919184049,-5.95722124393312));
#28422=CARTESIAN_POINT('Ctrl Pts',(-7.60054746639873,17.2799782900503,-5.62509800356719));
#28423=CARTESIAN_POINT('Ctrl Pts',(-7.56012110045393,16.3594808325921,-5.48933294767266));
#28424=CARTESIAN_POINT('Ctrl Pts',(-8.34172744353445,15.9507491910813,-5.1881086499226));
#28425=CARTESIAN_POINT('Ctrl Pts',(-7.49539872629226,17.3451970522154,-5.3043111217849));
#28426=CARTESIAN_POINT('Ctrl Pts',(-7.44265254159941,16.413527382139,-5.15230673839765));
#28427=CARTESIAN_POINT('Ctrl Pts',(-8.22632494925749,16.0109511247932,-4.80670062525685));
#28428=CARTESIAN_POINT('Ctrl Pts',(-7.24864440937974,17.4928269391644,-4.68606340046019));
#28429=CARTESIAN_POINT('Ctrl Pts',(-7.16932337182266,16.5345111926349,-4.50736742998995));
#28430=CARTESIAN_POINT('Ctrl Pts',(-7.95550797735527,16.1472248672498,-4.07161868859358));
#28431=CARTESIAN_POINT('Ctrl Pts',(-7.10730366773621,17.5750930730766,-4.38813130745318));
#28432=CARTESIAN_POINT('Ctrl Pts',(-7.01301294517219,16.6016115427834,-4.19830815404623));
#28433=CARTESIAN_POINT('Ctrl Pts',(-7.80038415841105,16.2231628362877,-3.71738446795083));
#28434=CARTESIAN_POINT('Ctrl Pts',(-6.78976913329141,17.7516792840673,-3.81308262809748));
#28435=CARTESIAN_POINT('Ctrl Pts',(-6.66526779473809,16.7437872397752,-3.60691491129501));
#28436=CARTESIAN_POINT('Ctrl Pts',(-7.45188471830734,16.3861654933836,-3.03366517195585));
#28437=CARTESIAN_POINT('Ctrl Pts',(-6.61357326878162,17.8460111736686,-3.53596957548935));
#28438=CARTESIAN_POINT('Ctrl Pts',(-6.47301642497377,16.8191166151697,-3.32428492883157));
#28439=CARTESIAN_POINT('Ctrl Pts',(-7.25850682191698,16.4732410829151,-2.70418429828093));
#28440=CARTESIAN_POINT('Ctrl Pts',(-6.22536744072326,18.0423400532628,-3.00215586940299));
#28441=CARTESIAN_POINT('Ctrl Pts',(-6.05435246414523,16.9734934471226,-2.7856742472814));
#28442=CARTESIAN_POINT('Ctrl Pts',(-6.83244445950206,16.6544677419447,-2.0694924117879));
#28443=CARTESIAN_POINT('Ctrl Pts',(-6.01671476286826,18.1425966890778,-2.75014226738085));
#28444=CARTESIAN_POINT('Ctrl Pts',(-5.83087248062031,17.0512960564225,-2.53450877806538));
#28445=CARTESIAN_POINT('Ctrl Pts',(-6.6034446698575,16.7470123279823,-1.76985419200821));
#28446=CARTESIAN_POINT('Ctrl Pts',(-5.35036565224163,18.4418170514269,-2.03834618162601));
#28447=CARTESIAN_POINT('Ctrl Pts',(-5.12056163117185,17.2814504145844,-1.82792133257243));
#28448=CARTESIAN_POINT('Ctrl Pts',(-5.87211542254812,17.0232157405731,-0.923545459877607));
#28449=CARTESIAN_POINT('Ctrl Pts',(-4.85205601954726,18.6397954432763,-1.62068622715121));
#28450=CARTESIAN_POINT('Ctrl Pts',(-4.60212559172194,17.4267808683366,-1.4316314270215));
#28451=CARTESIAN_POINT('Ctrl Pts',(-5.32524721431279,17.2059555554684,-0.426981969186781));
#28452=CARTESIAN_POINT('Ctrl Pts',(-4.29373077449685,18.8198698188909,-1.26158940397351));
#28453=CARTESIAN_POINT('Ctrl Pts',(-4.05040020405459,17.5517750653646,-1.10508701472557));
#28454=CARTESIAN_POINT('Ctrl Pts',(-4.71244104384512,17.3721875251301,-1.06752213906266E-15));
#28455=CARTESIAN_POINT('Ctrl Pts',(-4.26261338778693,18.0849267018157,-14.875));
#28456=CARTESIAN_POINT('Ctrl Pts',(-4.36728621357164,18.0345646349843,-14.8238231458034));
#28457=CARTESIAN_POINT('Ctrl Pts',(-4.47066603984279,17.9836961344339,-14.7713160666174));
#28458=CARTESIAN_POINT('Ctrl Pts',(-4.57293726166006,17.9323320438858,-14.7174958178478));
#28459=CARTESIAN_POINT('Ctrl Pts',(-4.67146734523438,17.8828468803716,-14.6656443437476));
#28460=CARTESIAN_POINT('Ctrl Pts',(-4.76896783203404,17.8329013817977,-14.6125734014967));
#28461=CARTESIAN_POINT('Ctrl Pts',(-4.86557698809706,17.7825339109652,-14.5583260017153));
#28462=CARTESIAN_POINT('Ctrl Pts',(-4.95543150101896,17.7356879934228,-14.5078714290509));
#28463=CARTESIAN_POINT('Ctrl Pts',(-5.04451439001857,17.6884769511579,-14.4563988610072));
#28464=CARTESIAN_POINT('Ctrl Pts',(-5.13292189721992,17.6409596293802,-14.4039733608045));
#28465=CARTESIAN_POINT('Ctrl Pts',(-5.21778196059643,17.5953489899085,-14.353651488708));
#28466=CARTESIAN_POINT('Ctrl Pts',(-5.30201934606125,17.549455956929,-14.3024512486777));
#28467=CARTESIAN_POINT('Ctrl Pts',(-5.38571159587319,17.503361604272,-14.2504642311565));
#28468=CARTESIAN_POINT('Ctrl Pts',(-5.46816101792737,17.4579517515669,-14.1992492195087));
#28469=CARTESIAN_POINT('Ctrl Pts',(-5.55008099149818,17.4123461809608,-14.1472700900238));
#28470=CARTESIAN_POINT('Ctrl Pts',(-5.63154386899368,17.3666552413443,-14.0946549924496));
#28471=CARTESIAN_POINT('Ctrl Pts',(-5.70699601269251,17.3243356051166,-14.0459220968665));
#28472=CARTESIAN_POINT('Ctrl Pts',(-5.78205573161066,17.281942771358,-13.996643579046));
#28473=CARTESIAN_POINT('Ctrl Pts',(-5.85678370662441,17.239594274303,-13.9469596296543));
#28474=CARTESIAN_POINT('Ctrl Pts',(-5.86273675107024,17.2362206717781,-13.943001663994));
#28475=CARTESIAN_POINT('Ctrl Pts',(-5.86868769334399,17.2328473673154,-13.9390411472596));
#28476=CARTESIAN_POINT('Ctrl Pts',(-5.87463656592348,17.2294744291862,-13.9350781619607));
#28477=CARTESIAN_POINT('Ctrl Pts',(-5.94218023588408,17.191177992886,-13.8900823131659));
#28478=CARTESIAN_POINT('Ctrl Pts',(-6.00952609799308,17.1528912123609,-13.8447109072821));
#28479=CARTESIAN_POINT('Ctrl Pts',(-6.07672203282712,17.1147265085998,-13.7991041023221));
#28480=CARTESIAN_POINT('Ctrl Pts',(-6.15303774324791,17.0713821234412,-13.7473075802685));
#28481=CARTESIAN_POINT('Ctrl Pts',(-6.2291789019832,17.028143489955,-13.6951247404768));
#28482=CARTESIAN_POINT('Ctrl Pts',(-6.3052620006147,16.9851285038395,-13.6426434530328));
#28483=CARTESIAN_POINT('Ctrl Pts',(-6.37709936525376,16.9445139219139,-13.5930908263568));
#28484=CARTESIAN_POINT('Ctrl Pts',(-6.44888463340197,16.9040987380384,-13.5432721433623));
#28485=CARTESIAN_POINT('Ctrl Pts',(-6.52074248491161,16.8640091075666,-13.493287537862));
#28486=CARTESIAN_POINT('Ctrl Pts',(-6.56132078321264,16.8413703986449,-13.4650611131939));
#28487=CARTESIAN_POINT('Ctrl Pts',(-6.60192274095193,16.8188359974411,-13.4367822566398));
#28488=CARTESIAN_POINT('Ctrl Pts',(-6.64257554275894,16.796432756076,-13.4084730253669));
#28489=CARTESIAN_POINT('Ctrl Pts',(-6.69153287005825,16.7694529964698,-13.3743808044272));
#28490=CARTESIAN_POINT('Ctrl Pts',(-6.74051510505213,16.7426909854859,-13.3402725411418));
#28491=CARTESIAN_POINT('Ctrl Pts',(-6.78965858551745,16.7161549427323,-13.3061343214082));
#28492=CARTESIAN_POINT('Ctrl Pts',(-6.84639050240779,16.6855213661553,-13.2667246860635));
#28493=CARTESIAN_POINT('Ctrl Pts',(-6.90327078439721,16.6552315277651,-13.2273240337237));
#28494=CARTESIAN_POINT('Ctrl Pts',(-6.96040712452314,16.6253536648596,-13.1879499262547));
#28495=CARTESIAN_POINT('Ctrl Pts',(-7.01594310573958,16.5963126652182,-13.1496786668776));
#28496=CARTESIAN_POINT('Ctrl Pts',(-7.07172086790775,16.5676606663574,-13.1114322899907));
#28497=CARTESIAN_POINT('Ctrl Pts',(-7.12782742604058,16.53949584061,-13.0732565035772));
#28498=CARTESIAN_POINT('Ctrl Pts',(-7.18144394311299,16.5125809858982,-13.0367749803451));
#28499=CARTESIAN_POINT('Ctrl Pts',(-7.23536057166625,16.4861109191502,-13.0003578234135));
#28500=CARTESIAN_POINT('Ctrl Pts',(-7.28964430395286,16.4602063421967,-12.9640742821639));
#28501=CARTESIAN_POINT('Ctrl Pts',(-7.33422861681448,16.4389303960745,-12.9342738854951));
#28502=CARTESIAN_POINT('Ctrl Pts',(-7.37906038061696,16.4180364302088,-12.9045640536257));
#28503=CARTESIAN_POINT('Ctrl Pts',(-7.42417289637397,16.3976113139917,-12.8750000000016));
#28504=CARTESIAN_POINT('',(-4.26261338778694,18.0849267018156,-1.));
#28505=CARTESIAN_POINT('Ctrl Pts',(-7.42417289637476,16.3976113139913,-2.99999999999997));
#28506=CARTESIAN_POINT('Ctrl Pts',(-7.36225162017796,16.4256467547421,-2.9594204869925));
#28507=CARTESIAN_POINT('Ctrl Pts',(-7.30094639302506,16.4545320426463,-2.91856077264145));
#28508=CARTESIAN_POINT('Ctrl Pts',(-7.24009139466157,16.4840912218767,-2.87754225192893));
#28509=CARTESIAN_POINT('Ctrl Pts',(-7.17579663629178,16.5153212003063,-2.83420520569084));
#28510=CARTESIAN_POINT('Ctrl Pts',(-7.11200471900219,16.5473033441628,-2.79069093814931));
#28511=CARTESIAN_POINT('Ctrl Pts',(-7.0485616279854,16.5798620319354,-2.7471168659627));
#28512=CARTESIAN_POINT('Ctrl Pts',(-6.98025522115035,16.614916549888,-2.70020256442825));
#28513=CARTESIAN_POINT('Ctrl Pts',(-6.91235344327022,16.6506392229992,-2.6532190682628));
#28514=CARTESIAN_POINT('Ctrl Pts',(-6.84470667791444,16.6868488321288,-2.60628234162304));
#28515=CARTESIAN_POINT('Ctrl Pts',(-6.77705991255867,16.7230584412584,-2.55934561498327));
#28516=CARTESIAN_POINT('Ctrl Pts',(-6.70966889386636,16.7597552671119,-2.51245542708785));
#28517=CARTESIAN_POINT('Ctrl Pts',(-6.64241644149763,16.7967930910134,-2.46569962889185));
#28518=CARTESIAN_POINT('Ctrl Pts',(-6.57233897132334,16.8353867319642,-2.41697979878676));
#28519=CARTESIAN_POINT('Ctrl Pts',(-6.50242163172557,16.8743437912577,-2.36840493401875));
#28520=CARTESIAN_POINT('Ctrl Pts',(-6.43251652697519,16.9135581508364,-2.32002298020697));
#28521=CARTESIAN_POINT('Ctrl Pts',(-6.35931673623709,16.954620715943,-2.26936074449228));
#28522=CARTESIAN_POINT('Ctrl Pts',(-6.28613110409549,16.9959654768125,-2.21890999430885));
#28523=CARTESIAN_POINT('Ctrl Pts',(-6.21280023886862,17.0375148551584,-2.16869022735185));
#28524=CARTESIAN_POINT('Ctrl Pts',(-6.16969661589326,17.0619374326576,-2.13917122612192));
#28525=CARTESIAN_POINT('Ctrl Pts',(-6.1265429451081,17.086431526281,-2.10973137070173));
#28526=CARTESIAN_POINT('Ctrl Pts',(-6.08330688289705,17.1109878358769,-2.08036939653045));
#28527=CARTESIAN_POINT('Ctrl Pts',(-6.0136392668642,17.1505561837009,-2.03305753143629));
#28528=CARTESIAN_POINT('Ctrl Pts',(-5.94390732283454,17.1902010442598,-1.98606424901363));
#28529=CARTESIAN_POINT('Ctrl Pts',(-5.87395832483882,17.2298569422314,-1.93947238083718));
#28530=CARTESIAN_POINT('Ctrl Pts',(-5.79682337542196,17.2735867421107,-1.88809406952459));
#28531=CARTESIAN_POINT('Ctrl Pts',(-5.71935440939585,17.3173647772406,-1.83714744008263));
#28532=CARTESIAN_POINT('Ctrl Pts',(-5.64148146818277,17.3610636873807,-1.7867839666029));
#28533=CARTESIAN_POINT('Ctrl Pts',(-5.56016891276116,17.4066927595241,-1.73419596023313));
#28534=CARTESIAN_POINT('Ctrl Pts',(-5.47841625448937,17.4522357096599,-1.68224347506384));
#28535=CARTESIAN_POINT('Ctrl Pts',(-5.39614987878206,17.4975832947874,-1.6310529385569));
#28536=CARTESIAN_POINT('Ctrl Pts',(-5.31003429924489,17.5450526714348,-1.57746722166816));
#28537=CARTESIAN_POINT('Ctrl Pts',(-5.22335621422618,17.5923081415182,-1.52471609071066));
#28538=CARTESIAN_POINT('Ctrl Pts',(-5.13603166624492,17.6392602637631,-1.47290009966545));
#28539=CARTESIAN_POINT('Ctrl Pts',(-5.04252759392154,17.6895349543925,-1.41741734840933));
#28540=CARTESIAN_POINT('Ctrl Pts',(-4.94828288017069,17.7394619360643,-1.36300648878106));
#28541=CARTESIAN_POINT('Ctrl Pts',(-4.8531872765823,17.7889697057021,-1.30974583887355));
#28542=CARTESIAN_POINT('Ctrl Pts',(-4.75201030281837,17.8416435005015,-1.25307916686139));
#28543=CARTESIAN_POINT('Ctrl Pts',(-4.64987085960817,17.893842962125,-1.19771403654983));
#28544=CARTESIAN_POINT('Ctrl Pts',(-4.54661799837511,17.9455214136771,-1.14370160718567));
#28545=CARTESIAN_POINT('Ctrl Pts',(-4.45291076337046,17.9924222428302,-1.09468257419079));
#28546=CARTESIAN_POINT('Ctrl Pts',(-4.35828650491551,18.0388947361867,-1.04677669805056));
#28547=CARTESIAN_POINT('Ctrl Pts',(-4.26261338778692,18.0849267018156,-1.00000000000002));
#28548=CARTESIAN_POINT('Origin',(-5.10514446416555,18.8198698188909,0.));
#28549=CARTESIAN_POINT('Ctrl Pts',(-4.33449582597651,18.8064455740235,-1.28798683503108));
#28550=CARTESIAN_POINT('Ctrl Pts',(-4.21041218740497,18.1927840286017,-1.2071616648505));
#28551=CARTESIAN_POINT('Ctrl Pts',(-4.3700807197326,17.7637855531036,-0.772531983761533));
#28552=CARTESIAN_POINT('Ctrl Pts',(-4.00042123744047,18.9207316512653,-1.07018515119445));
#28553=CARTESIAN_POINT('Ctrl Pts',(-3.94435406442238,18.3471385657429,-1.04232225428572));
#28554=CARTESIAN_POINT('Ctrl Pts',(-4.08161076289601,17.9187745448053,-0.684948449715675));
#28555=CARTESIAN_POINT('Ctrl Pts',(-3.64551666608151,18.9604224970613,-0.875159857664685));
#28556=CARTESIAN_POINT('Ctrl Pts',(-3.63144227316264,18.4451127783963,-0.869290948000206));
#28557=CARTESIAN_POINT('Ctrl Pts',(-3.75476449736778,18.0355093239667,-0.580889520521902));
#28558=CARTESIAN_POINT('Ctrl Pts',(-2.92607962857381,18.9432173241546,-0.548888115088505));
#28559=CARTESIAN_POINT('Ctrl Pts',(-2.96645048635243,18.5378314306372,-0.566779801034313));
#28560=CARTESIAN_POINT('Ctrl Pts',(-3.06702439599705,18.185370762247,-0.389458929501563));
#28561=CARTESIAN_POINT('Ctrl Pts',(-2.55821923863767,18.8884652562902,-0.413977802884962));
#28562=CARTESIAN_POINT('Ctrl Pts',(-2.61131053681094,18.5396309401508,-0.432068222184205));
#28563=CARTESIAN_POINT('Ctrl Pts',(-2.70267013757716,18.2245847168884,-0.299660180936123));
#28564=CARTESIAN_POINT('Ctrl Pts',(-1.82891451879158,18.7188973096676,-0.204263613546989));
#28565=CARTESIAN_POINT('Ctrl Pts',(-1.89153943192661,18.4751292208516,-0.21954016975466));
#28566=CARTESIAN_POINT('Ctrl Pts',(-1.96287487083709,18.2420370452619,-0.154945093056182));
#28567=CARTESIAN_POINT('Ctrl Pts',(-1.46353131432072,18.6039976779118,-0.127285834606972));
#28568=CARTESIAN_POINT('Ctrl Pts',(-1.52010388032437,18.4109076718901,-0.137307211669863));
#28569=CARTESIAN_POINT('Ctrl Pts',(-1.58083477323453,18.2227697776629,-0.0973283859171704));
#28570=CARTESIAN_POINT('Ctrl Pts',(-0.729117484549751,18.3301937948767,
-0.0248672136816333));
#28571=CARTESIAN_POINT('Ctrl Pts',(-0.765887787240446,18.2357095390217,
-0.027895363559901));
#28572=CARTESIAN_POINT('Ctrl Pts',(-0.800159021641761,18.1403975455722,
-0.0200632859980195));
#28573=CARTESIAN_POINT('Ctrl Pts',(-0.361264579836653,18.1710404144961,
-1.27030416149535E-14));
#28574=CARTESIAN_POINT('Ctrl Pts',(-0.37996820254999,18.1240305403966,-2.39037871064658E-13));
#28575=CARTESIAN_POINT('Ctrl Pts',(-0.398736372182772,18.0770350537363,
-4.65437000046116E-13));
#28576=CARTESIAN_POINT('Ctrl Pts',(9.87716250982808E-14,18.,-2.01661604082304E-14));
#28577=CARTESIAN_POINT('Ctrl Pts',(9.87716250982808E-14,18.,-2.01661604082304E-14));
#28578=CARTESIAN_POINT('Ctrl Pts',(9.87716250982808E-14,18.,-2.01661604082304E-14));
#28579=CARTESIAN_POINT('Ctrl Pts',(-4.26261338778694,18.0849267018156,-1.));
#28580=CARTESIAN_POINT('Ctrl Pts',(-3.95178714242432,18.188266342333,-0.814067986447267));
#28581=CARTESIAN_POINT('Ctrl Pts',(-3.61923443569505,18.2429627164578,-0.657679757707574));
#28582=CARTESIAN_POINT('Ctrl Pts',(-3.09548155756287,18.2860517458272,-0.463235421761033));
#28583=CARTESIAN_POINT('Ctrl Pts',(-2.91664062652111,18.2933512364511,-0.405102243904273));
#28584=CARTESIAN_POINT('Ctrl Pts',(-2.55896263908653,18.2964774327613,-0.302902733783915));
#28585=CARTESIAN_POINT('Ctrl Pts',(-2.37912173967015,18.2923841267789,-0.25843996217478));
#28586=CARTESIAN_POINT('Ctrl Pts',(-1.83693290496405,18.2663432658697,-0.142343866931082));
#28587=CARTESIAN_POINT('Ctrl Pts',(-1.47194228891689,18.2307806146047,-0.0878435449572992));
#28588=CARTESIAN_POINT('Ctrl Pts',(-0.735959210913743,18.1331323295489,
-0.0164961393612659));
#28589=CARTESIAN_POINT('Ctrl Pts',(-0.364750325439687,18.0705479584028,
-6.57768140928924E-16));
#28590=CARTESIAN_POINT('Ctrl Pts',(1.11022302462516E-13,18.,0.));
#28591=CARTESIAN_POINT('Ctrl Pts',(4.3700355726488,17.7638095491918,-0.772517910421123));
#28592=CARTESIAN_POINT('Ctrl Pts',(4.21037028349325,18.1928079867522,-1.2071356280258));
#28593=CARTESIAN_POINT('Ctrl Pts',(4.33444454890457,18.8064629622356,-1.28795340497675));
#28594=CARTESIAN_POINT('Ctrl Pts',(4.08157677842179,17.9187863941712,-0.68493732529669));
#28595=CARTESIAN_POINT('Ctrl Pts',(3.94432134460992,18.3471485006655,-1.0423041033654));
#28596=CARTESIAN_POINT('Ctrl Pts',(4.00038492840469,18.9207355731398,-1.07016519964085));
#28597=CARTESIAN_POINT('Ctrl Pts',(3.75474604679998,18.035513052921,-0.58088413905726));
#28598=CARTESIAN_POINT('Ctrl Pts',(3.63142428278685,18.4451150132921,-0.869282717230128));
#28599=CARTESIAN_POINT('Ctrl Pts',(3.64549788807283,18.9604219221275,-0.875151341779449));
#28600=CARTESIAN_POINT('Ctrl Pts',(3.06702447289767,18.1853704927497,-0.389458793918743));
#28601=CARTESIAN_POINT('Ctrl Pts',(2.96645051656865,18.5378312165733,-0.566779784268469));
#28602=CARTESIAN_POINT('Ctrl Pts',(2.9260796388088,18.9432172213792,-0.54888811962447));
#28603=CARTESIAN_POINT('Ctrl Pts',(2.7026702075431,18.2245844756192,-0.299660079535286));
#28604=CARTESIAN_POINT('Ctrl Pts',(2.61131057064228,18.5396307565727,-0.432068211521341));
#28605=CARTESIAN_POINT('Ctrl Pts',(2.55821925230454,18.8884651665002,-0.413977807541778));
#28606=CARTESIAN_POINT('Ctrl Pts',(1.96287492560049,18.242036866318,-0.15494504346654));
#28607=CARTESIAN_POINT('Ctrl Pts',(1.8915394662703,18.4751290932002,-0.219540167032862));
#28608=CARTESIAN_POINT('Ctrl Pts',(1.82891453529854,18.7188972454107,-0.204263617573607));
#28609=CARTESIAN_POINT('Ctrl Pts',(1.5808348198991,18.2227696331009,-0.0973283551978142));
#28610=CARTESIAN_POINT('Ctrl Pts',(1.52010391064048,18.410907571007,-0.137307210178231));
#28611=CARTESIAN_POINT('Ctrl Pts',(1.46353132936822,18.6039976265544,-0.127285837272504));
#28612=CARTESIAN_POINT('Ctrl Pts',(0.800159048007738,18.1403974722464,-0.0200632799728283));
#28613=CARTESIAN_POINT('Ctrl Pts',(0.765887806062742,18.235709489677,-0.027895363671069));
#28614=CARTESIAN_POINT('Ctrl Pts',(0.729117494448843,18.3301937694396,-0.0248672144968317));
#28615=CARTESIAN_POINT('Ctrl Pts',(0.398736386626917,18.0770350175674,-6.65308014686413E-13));
#28616=CARTESIAN_POINT('Ctrl Pts',(0.379968212283047,18.1240305159575,-3.43198578914328E-13));
#28617=CARTESIAN_POINT('Ctrl Pts',(0.361264584891461,18.1710404017938,-2.11825291438926E-14));
#28618=CARTESIAN_POINT('Ctrl Pts',(9.87716271744808E-14,18.,-2.01661604082304E-14));
#28619=CARTESIAN_POINT('Ctrl Pts',(9.87716271744808E-14,18.,-2.01661604082304E-14));
#28620=CARTESIAN_POINT('Ctrl Pts',(9.87716271744808E-14,18.,-2.01661604082304E-14));
#28621=CARTESIAN_POINT('',(4.26261338778694,18.0849267018156,-1.));
#28622=CARTESIAN_POINT('Ctrl Pts',(1.11022302462516E-13,18.,0.));
#28623=CARTESIAN_POINT('Ctrl Pts',(0.733684917774343,18.141905678209,-8.43898925349459E-15));
#28624=CARTESIAN_POINT('Ctrl Pts',(1.47554802668048,18.248989994314,-0.0649575167164615));
#28625=CARTESIAN_POINT('Ctrl Pts',(2.37917217060933,18.292385615839,-0.258451979040235));
#28626=CARTESIAN_POINT('Ctrl Pts',(2.5590083227402,18.2964779051253,-0.302914725119498));
#28627=CARTESIAN_POINT('Ctrl Pts',(2.91667689706811,18.2933500475868,-0.405113669626746));
#28628=CARTESIAN_POINT('Ctrl Pts',(3.09551309904672,18.2860499025368,-0.463246299412621));
#28629=CARTESIAN_POINT('Ctrl Pts',(3.61925135711831,18.2429598209236,-0.657687704390198));
#28630=CARTESIAN_POINT('Ctrl Pts',(3.95179505566489,18.1882637114373,-0.814072720039597));
#28631=CARTESIAN_POINT('Ctrl Pts',(4.26261338778694,18.0849267018156,-1.));
#28632=CARTESIAN_POINT('Origin',(5.10514446416566,18.8198698188909,0.));
#28633=CARTESIAN_POINT('Ctrl Pts',(4.29373077449695,18.8198698188909,-1.2615894039735));
#28634=CARTESIAN_POINT('Ctrl Pts',(4.05040020405469,17.5517750653646,-1.10508701472556));
#28635=CARTESIAN_POINT('Ctrl Pts',(4.71244104384522,17.3721875251301,-1.06752213906265E-15));
#28636=CARTESIAN_POINT('Ctrl Pts',(4.85172205448711,18.6399031556679,-1.62047143157596));
#28637=CARTESIAN_POINT('Ctrl Pts',(4.60179941708484,17.4268547636714,-1.43143837716499));
#28638=CARTESIAN_POINT('Ctrl Pts',(5.32488118013602,17.2060548471941,-0.426726929314143));
#28639=CARTESIAN_POINT('Ctrl Pts',(5.35047866129667,18.4418014142624,-2.03831036656378));
#28640=CARTESIAN_POINT('Ctrl Pts',(5.12064004592513,17.2814545873287,-1.82783948434398));
#28641=CARTESIAN_POINT('Ctrl Pts',(5.87223945189375,17.0232013062603,-0.923502876585836));
#28642=CARTESIAN_POINT('Ctrl Pts',(6.01799603717822,18.1420037326857,-2.75158942970812));
#28643=CARTESIAN_POINT('Ctrl Pts',(5.8322275983878,17.050842485112,-2.53593507991418));
#28644=CARTESIAN_POINT('Ctrl Pts',(6.60485088974162,16.7464649836239,-1.7715748338448));
#28645=CARTESIAN_POINT('Ctrl Pts',(6.22802018553555,18.0410299920564,-3.00559364749459));
#28646=CARTESIAN_POINT('Ctrl Pts',(6.05721596844273,16.9724647253118,-2.7891413201072));
#28647=CARTESIAN_POINT('Ctrl Pts',(6.83535589111342,16.6532584546769,-2.07357984873547));
#28648=CARTESIAN_POINT('Ctrl Pts',(6.61444355976506,17.8455392272447,-3.53737817259522));
#28649=CARTESIAN_POINT('Ctrl Pts',(6.47397956801548,16.818734456234,-3.32573967378444));
#28650=CARTESIAN_POINT('Ctrl Pts',(7.25946198077314,16.4728054400626,-2.70585908696185));
#28651=CARTESIAN_POINT('Ctrl Pts',(6.78984519594625,17.7516276808024,-3.81332671967964));
#28652=CARTESIAN_POINT('Ctrl Pts',(6.66536331485447,16.7437399954122,-3.60718861993155));
#28653=CARTESIAN_POINT('Ctrl Pts',(7.45196819833014,16.3861178595996,-3.0339553910857));
#28654=CARTESIAN_POINT('Ctrl Pts',(7.10602320700696,17.5758144266797,-4.38570647946684));
#28655=CARTESIAN_POINT('Ctrl Pts',(7.01161694949589,16.6021903559513,-4.19582456913687));
#28656=CARTESIAN_POINT('Ctrl Pts',(7.79897883144043,16.2238287011531,-3.71450140474986));
#28657=CARTESIAN_POINT('Ctrl Pts',(7.24680107601194,17.4939013437499,-4.68213458785877));
#28658=CARTESIAN_POINT('Ctrl Pts',(7.16729424914682,16.53538393131,-4.5033073042272));
#28659=CARTESIAN_POINT('Ctrl Pts',(7.9534848882684,16.1482166253277,-4.0669474232218));
#28660=CARTESIAN_POINT('Ctrl Pts',(7.4927351377619,17.3468185637659,-5.29696029054636));
#28661=CARTESIAN_POINT('Ctrl Pts',(7.43969881407855,16.4148594991966,-5.14462969386339));
#28662=CARTESIAN_POINT('Ctrl Pts',(8.22340161649126,16.0124479046869,-4.79796066055123));
#28663=CARTESIAN_POINT('Ctrl Pts',(7.59843488959468,17.2812951267931,-5.61809528199464));
#28664=CARTESIAN_POINT('Ctrl Pts',(7.55776347710494,16.3605717978334,-5.48196671762775));
#28665=CARTESIAN_POINT('Ctrl Pts',(8.3394088551856,15.9519647326952,-5.17978257942572));
#28666=CARTESIAN_POINT('Ctrl Pts',(7.85078664959272,17.1222147255282,-6.5896000401223));
#28667=CARTESIAN_POINT('Ctrl Pts',(7.83853818368898,16.2290439809763,-6.50196528014747));
#28668=CARTESIAN_POINT('Ctrl Pts',(8.61636911516069,15.8051212845613,-6.33487878776941));
#28669=CARTESIAN_POINT('Ctrl Pts',(7.93672823551223,17.0646099827074,-7.25148511305119));
#28670=CARTESIAN_POINT('Ctrl Pts',(7.93663307907031,16.1799952820739,-7.20918238147577));
#28671=CARTESIAN_POINT('Ctrl Pts',(8.710691437893,15.751947676348,-7.1218445044932));
#28672=CARTESIAN_POINT('Ctrl Pts',(7.93768657939644,17.0639797987105,-8.09776804418832));
#28673=CARTESIAN_POINT('Ctrl Pts',(7.93770957586298,16.1794674107193,-8.10764417924993));
#28674=CARTESIAN_POINT('Ctrl Pts',(8.71174323535012,15.7513659680398,-8.12805491868078));
#28675=CARTESIAN_POINT('Ctrl Pts',(7.93240014505281,17.0674607979061,-8.26866275408054));
#28676=CARTESIAN_POINT('Ctrl Pts',(7.93176509524196,16.1823866550743,-8.28915283131846));
#28677=CARTESIAN_POINT('Ctrl Pts',(8.70594128558497,15.7545791980315,-8.33124469184719));
#28678=CARTESIAN_POINT('Ctrl Pts',(7.91102975013306,17.0814770208683,-8.6070140950225));
#28679=CARTESIAN_POINT('Ctrl Pts',(7.90776940619277,16.1941201670182,-8.64818951047776));
#28680=CARTESIAN_POINT('Ctrl Pts',(8.68248692160874,15.767517250068,-8.7335364437005));
#28681=CARTESIAN_POINT('Ctrl Pts',(7.89499158493914,17.0919817317593,-8.77489499114022));
#28682=CARTESIAN_POINT('Ctrl Pts',(7.8897489782093,16.2029188357821,-8.82632296847022));
#28683=CARTESIAN_POINT('Ctrl Pts',(8.66488476781437,15.7772139061692,-8.9331428634661));
#28684=CARTESIAN_POINT('Ctrl Pts',(7.83124885358606,17.1334594467781,-9.27477806868774));
#28685=CARTESIAN_POINT('Ctrl Pts',(7.81819429110603,16.2376097544146,-9.35647171304077));
#28686=CARTESIAN_POINT('Ctrl Pts',(8.59492605886999,15.8155010279355,-9.52749203445515));
#28687=CARTESIAN_POINT('Ctrl Pts',(7.767980844109,17.1743995785599,-9.6030324637013));
#28688=CARTESIAN_POINT('Ctrl Pts',(7.74705485466677,16.2718853507128,-9.70416044777262));
#28689=CARTESIAN_POINT('Ctrl Pts',(8.52548836424224,15.8532919184051,-9.91777875606642));
#28690=CARTESIAN_POINT('Ctrl Pts',(7.6005474663986,17.2799782900502,-10.2499019964334));
#28691=CARTESIAN_POINT('Ctrl Pts',(7.56012110045394,16.3594808325921,-10.3856670523278));
#28692=CARTESIAN_POINT('Ctrl Pts',(8.34172744353473,15.9507491910812,-10.686891350078));
#28693=CARTESIAN_POINT('Ctrl Pts',(7.49539872629229,17.3451970522147,-10.5706888782151));
#28694=CARTESIAN_POINT('Ctrl Pts',(7.44265254159908,16.413527382139,-10.722693261602));
#28695=CARTESIAN_POINT('Ctrl Pts',(8.22632494925752,16.0109511247932,-11.0682993747428));
#28696=CARTESIAN_POINT('Ctrl Pts',(7.24864440937976,17.4928269391651,-11.1889365995399));
#28697=CARTESIAN_POINT('Ctrl Pts',(7.16932337182303,16.5345111926349,-11.3676325700104));
#28698=CARTESIAN_POINT('Ctrl Pts',(7.95550797735529,16.1472248672497,-11.8033813114068));
#28699=CARTESIAN_POINT('Ctrl Pts',(7.10730366773597,17.5750930730772,-11.4868686925473));
#28700=CARTESIAN_POINT('Ctrl Pts',(7.01301294517187,16.6016115427848,-11.6766918459536));
#28701=CARTESIAN_POINT('Ctrl Pts',(7.80038415841053,16.223162836288,-12.1576155320495));
#28702=CARTESIAN_POINT('Ctrl Pts',(6.78976913329171,17.7516792840666,-12.0619173719021));
#28703=CARTESIAN_POINT('Ctrl Pts',(6.66526779473846,16.7437872397738,-12.2680850887052));
#28704=CARTESIAN_POINT('Ctrl Pts',(7.45188471830793,16.3861654933833,-12.8413348280438));
#28705=CARTESIAN_POINT('Ctrl Pts',(6.61357326878161,17.8460111736693,-12.3390304245107));
#28706=CARTESIAN_POINT('Ctrl Pts',(6.47301642497381,16.819116615169,-12.5507150711689));
#28707=CARTESIAN_POINT('Ctrl Pts',(7.25850682191717,16.473241082915,-13.1708157017191));
#28708=CARTESIAN_POINT('Ctrl Pts',(6.22536744072334,18.0423400532621,-12.872844130597));
#28709=CARTESIAN_POINT('Ctrl Pts',(6.05435246414527,16.9734934471233,-13.0893257527182));
#28710=CARTESIAN_POINT('Ctrl Pts',(6.83244445950195,16.6544677419447,-13.8055075882121));
#28711=CARTESIAN_POINT('Ctrl Pts',(6.01671476286829,18.1425966890777,-13.1248577326192));
#28712=CARTESIAN_POINT('Ctrl Pts',(5.83087248062037,17.0512960564225,-13.3404912219347));
#28713=CARTESIAN_POINT('Ctrl Pts',(6.60344466985757,16.7470123279822,-14.1051458079917));
#28714=CARTESIAN_POINT('Ctrl Pts',(5.35036565224178,18.4418170514269,-13.8366538183739));
#28715=CARTESIAN_POINT('Ctrl Pts',(5.12056163117187,17.2814504145844,-14.0470786674275));
#28716=CARTESIAN_POINT('Ctrl Pts',(5.87211542254819,17.0232157405731,-14.9514545401227));
#28717=CARTESIAN_POINT('Ctrl Pts',(4.85205601950993,18.6397954431123,-14.2543137728728));
#28718=CARTESIAN_POINT('Ctrl Pts',(4.60212559171587,17.4267808681677,-14.4433685730329));
#28719=CARTESIAN_POINT('Ctrl Pts',(5.32524721434875,17.2059555554588,-15.4480180308682));
#28720=CARTESIAN_POINT('Ctrl Pts',(4.29373077449694,18.819869818891,-14.6134105960265));
#28721=CARTESIAN_POINT('Ctrl Pts',(4.05040020405468,17.5517750653647,-14.7699129852744));
#28722=CARTESIAN_POINT('Ctrl Pts',(4.71244104384522,17.3721875251302,-15.875));
#28723=CARTESIAN_POINT('Ctrl Pts',(4.26261338778696,18.0849267018155,-1.00000000000006));
#28724=CARTESIAN_POINT('Ctrl Pts',(4.36728621326876,18.0345646351299,-1.05117685404853));
#28725=CARTESIAN_POINT('Ctrl Pts',(4.47066603924481,17.9836961347291,-1.10368393307799));
#28726=CARTESIAN_POINT('Ctrl Pts',(4.57293726077334,17.9323320443341,-1.15750418168388));
#28727=CARTESIAN_POINT('Ctrl Pts',(4.67146734411905,17.8828468809424,-1.2093556556525));
#28728=CARTESIAN_POINT('Ctrl Pts',(4.76896783069495,17.8329013824936,-1.26242659776644));
#28729=CARTESIAN_POINT('Ctrl Pts',(4.86557698653789,17.7825339117877,-1.31667399740623));
#28730=CARTESIAN_POINT('Ctrl Pts',(4.95543149928796,17.735687994346,-1.36712856995748));
#28731=CARTESIAN_POINT('Ctrl Pts',(5.04451438811836,17.6884769521829,-1.41860113788473));
#28732=CARTESIAN_POINT('Ctrl Pts',(5.13292189515225,17.6409596305071,-1.47102663796827));
#28733=CARTESIAN_POINT('Ctrl Pts',(5.21778195838363,17.5953489911249,-1.52134850995953));
#28734=CARTESIAN_POINT('Ctrl Pts',(5.30201934370471,17.5494559582348,-1.57254874988241));
#28735=CARTESIAN_POINT('Ctrl Pts',(5.38571159337366,17.5033616056665,-1.62453576729421));
#28736=CARTESIAN_POINT('Ctrl Pts',(5.46816101585694,17.4579517527347,-1.6757507791882));
#28737=CARTESIAN_POINT('Ctrl Pts',(5.55008098985025,17.4123461818984,-1.72772990892807));
#28738=CARTESIAN_POINT('Ctrl Pts',(5.63154386776266,17.3666552420496,-1.78034500676327));
#28739=CARTESIAN_POINT('Ctrl Pts',(5.70699601133102,17.3243356058963,-1.82907790225456));
#28740=CARTESIAN_POINT('Ctrl Pts',(5.78205573011926,17.2819427722116,-1.87835641998092));
#28741=CARTESIAN_POINT('Ctrl Pts',(5.85678370500345,17.2395942752292,-1.92804036927623));
#28742=CARTESIAN_POINT('Ctrl Pts',(5.86273674999138,17.2362206723971,-1.93199833529621));
#28743=CARTESIAN_POINT('Ctrl Pts',(5.86868769280685,17.2328473676272,-1.93595885239063));
#28744=CARTESIAN_POINT('Ctrl Pts',(5.87463656592768,17.2294744291908,-1.93992183805002));
#28745=CARTESIAN_POINT('Ctrl Pts',(5.94218023588707,17.1911779928887,-1.98491768684271));
#28746=CARTESIAN_POINT('Ctrl Pts',(6.0095260979954,17.152891212362,-2.03028909272496));
#28747=CARTESIAN_POINT('Ctrl Pts',(6.07672203282924,17.1147265086007,-2.0758958976845));
#28748=CARTESIAN_POINT('Ctrl Pts',(6.15303774329964,17.0713821234137,-2.12769241977143));
#28749=CARTESIAN_POINT('Ctrl Pts',(6.22917890208468,17.0281434898988,-2.17987525959672));
#28750=CARTESIAN_POINT('Ctrl Pts',(6.30526200076612,16.9851285037549,-2.23235654707469));
#28751=CARTESIAN_POINT('Ctrl Pts',(6.37709936544756,16.9445139218052,-2.28190917377949));
#28752=CARTESIAN_POINT('Ctrl Pts',(6.44888463363832,16.9040987379059,-2.33172785680304));
#28753=CARTESIAN_POINT('Ctrl Pts',(6.52074248519078,16.8640091074109,-2.38171246233275));
#28754=CARTESIAN_POINT('Ctrl Pts',(6.56132078339888,16.8413703985416,-2.40993888693603));
#28755=CARTESIAN_POINT('Ctrl Pts',(6.60192274104519,16.8188359973897,-2.43821774342518));
#28756=CARTESIAN_POINT('Ctrl Pts',(6.64257554275894,16.796432756076,-2.46652697463318));
#28757=CARTESIAN_POINT('Ctrl Pts',(6.6915328700589,16.7694529964694,-2.5006191955733));
#28758=CARTESIAN_POINT('Ctrl Pts',(6.74051510505307,16.7426909854853,-2.5347274588589));
#28759=CARTESIAN_POINT('Ctrl Pts',(6.78965858551858,16.7161549427317,-2.56886567859258));
#28760=CARTESIAN_POINT('Ctrl Pts',(6.84639050239587,16.6855213661617,-2.60827531392821));
#28761=CARTESIAN_POINT('Ctrl Pts',(6.90327078437239,16.6552315277783,-2.64767596625816));
#28762=CARTESIAN_POINT('Ctrl Pts',(6.96040712448552,16.6253536648793,-2.68705007371724));
#28763=CARTESIAN_POINT('Ctrl Pts',(7.01594310569148,16.5963126652432,-2.72532133308595));
#28764=CARTESIAN_POINT('Ctrl Pts',(7.07172086784928,16.5676606663874,-2.7635677099645));
#28765=CARTESIAN_POINT('Ctrl Pts',(7.12782742597172,16.5394958406447,-2.80174349637038));
#28766=CARTESIAN_POINT('Ctrl Pts',(7.18144394303668,16.5125809859361,-2.83822501959682));
#28767=CARTESIAN_POINT('Ctrl Pts',(7.2353605715825,16.486110919191,-2.87464217652343));
#28768=CARTESIAN_POINT('Ctrl Pts',(7.28964430386149,16.4602063422403,-2.91092571776942));
#28769=CARTESIAN_POINT('Ctrl Pts',(7.33422861675332,16.438930396103,-2.94072611445956));
#28770=CARTESIAN_POINT('Ctrl Pts',(7.37906038058627,16.4180364302227,-2.97043594635113));
#28771=CARTESIAN_POINT('Ctrl Pts',(7.42417289637392,16.3976113139918,-2.99999999999845));
#28772=CARTESIAN_POINT('',(4.26261338778694,18.0849267018157,-14.875));
#28773=CARTESIAN_POINT('Ctrl Pts',(7.42417289637482,16.3976113139914,-12.875));
#28774=CARTESIAN_POINT('Ctrl Pts',(7.36225161991056,16.4256467548633,-12.915579513499));
#28775=CARTESIAN_POINT('Ctrl Pts',(7.30094639249221,16.4545320429019,-12.9564392282447));
#28776=CARTESIAN_POINT('Ctrl Pts',(7.24009139386733,16.4840912222715,-12.9974577492801));
#28777=CARTESIAN_POINT('Ctrl Pts',(7.1757966350601,16.5153212009266,-13.0407947959681));
#28778=CARTESIAN_POINT('Ctrl Pts',(7.11200471734016,16.547303345018,-13.0843090638802));
#28779=CARTESIAN_POINT('Ctrl Pts',(7.04856162589895,16.5798620330284,-13.1278831363843));
#28780=CARTESIAN_POINT('Ctrl Pts',(6.98025521941957,16.6149165508199,-13.1747974377025));
#28781=CARTESIAN_POINT('Ctrl Pts',(6.91235344189253,16.6506392237579,-13.2217809335886));
#28782=CARTESIAN_POINT('Ctrl Pts',(6.84470667688731,16.686848832706,-13.2687176599199));
#28783=CARTESIAN_POINT('Ctrl Pts',(6.77705991188208,16.7230584416542,-13.3156543862513));
#28784=CARTESIAN_POINT('Ctrl Pts',(6.70966889353779,16.7597552673182,-13.3625445738093));
#28785=CARTESIAN_POINT('Ctrl Pts',(6.64241644150871,16.7967930910297,-13.4093003716696));
#28786=CARTESIAN_POINT('Ctrl Pts',(6.57233897029021,16.8353867325524,-13.4580202023968));
#28787=CARTESIAN_POINT('Ctrl Pts',(6.50242162964476,16.8743437924329,-13.5065950677803));
#28788=CARTESIAN_POINT('Ctrl Pts',(6.43251652384589,16.9135581526054,-13.5549770222157));
#28789=CARTESIAN_POINT('Ctrl Pts',(6.35931673223419,16.9546207182078,-13.605639258428));
#28790=CARTESIAN_POINT('Ctrl Pts',(6.28613109921804,16.9959654795788,-13.6560900091192));
#28791=CARTESIAN_POINT('Ctrl Pts',(6.2128002331182,17.0375148584257,-13.7063097766082));
#28792=CARTESIAN_POINT('Ctrl Pts',(6.1696966120536,17.061937434846,-13.7358287764909));
#28793=CARTESIAN_POINT('Ctrl Pts',(6.12654294318534,17.0864315273824,-13.765268630581));
#28794=CARTESIAN_POINT('Ctrl Pts',(6.08330688290299,17.1109878358836,-13.7946306034417));
#28795=CARTESIAN_POINT('Ctrl Pts',(6.01363926687775,17.1505561837045,-13.8419424685295));
#28796=CARTESIAN_POINT('Ctrl Pts',(5.94390732285264,17.1902010442706,-13.8889357509433));
#28797=CARTESIAN_POINT('Ctrl Pts',(5.87395832485907,17.2298569422537,-13.9355276191119));
#28798=CARTESIAN_POINT('Ctrl Pts',(5.79682337621975,17.2735867417064,-13.9869059298996));
#28799=CARTESIAN_POINT('Ctrl Pts',(5.71935441097595,17.3173647764086,-14.0378525588354));
#28800=CARTESIAN_POINT('Ctrl Pts',(5.64148147055135,17.3610636861213,-14.088216031827));
#28801=CARTESIAN_POINT('Ctrl Pts',(5.56016891604116,17.406692757769,-14.1408040376301));
#28802=CARTESIAN_POINT('Ctrl Pts',(5.47841625868845,17.4522357074098,-14.1927565222537));
#28803=CARTESIAN_POINT('Ctrl Pts',(5.3961498839107,17.4975832920454,-14.2439470582352));
#28804=CARTESIAN_POINT('Ctrl Pts',(5.31003430543961,17.5450526681267,-14.2975327745159));
#28805=CARTESIAN_POINT('Ctrl Pts',(5.22335622149967,17.592308137648,-14.3502839048893));
#28806=CARTESIAN_POINT('Ctrl Pts',(5.13603167461429,17.6392602593379,-14.4020998953737));
#28807=CARTESIAN_POINT('Ctrl Pts',(5.04252760357117,17.6895349493158,-14.457582645966));
#28808=CARTESIAN_POINT('Ctrl Pts',(4.94828289112192,17.7394619303452,-14.5119935049597));
#28809=CARTESIAN_POINT('Ctrl Pts',(4.85318728886316,17.7889696993535,-14.5652541542623));
#28810=CARTESIAN_POINT('Ctrl Pts',(4.75201031666407,17.8416434934051,-14.6219208255467));
#28811=CARTESIAN_POINT('Ctrl Pts',(4.64987087505333,17.8938429542968,-14.6772859551681));
#28812=CARTESIAN_POINT('Ctrl Pts',(4.54661801546361,17.9455214051367,-14.7312983838822));
#28813=CARTESIAN_POINT('Ctrl Pts',(4.45291077487284,17.9924222371858,-14.7803174199895));
#28814=CARTESIAN_POINT('Ctrl Pts',(4.35828651072968,18.0388947333894,-14.8282232991068));
#28815=CARTESIAN_POINT('Ctrl Pts',(4.26261338778695,18.0849267018156,-14.8749999999999));
#28816=CARTESIAN_POINT('Origin',(5.10514446416566,18.819869818891,-15.875));
#28817=CARTESIAN_POINT('Ctrl Pts',(4.33449582574671,18.8064455741005,-14.5870131651188));
#28818=CARTESIAN_POINT('Ctrl Pts',(4.21041218730388,18.1927840291355,-14.6678383352104));
#28819=CARTESIAN_POINT('Ctrl Pts',(4.37008071934207,17.763785553718,-15.1024680157884));
#28820=CARTESIAN_POINT('Ctrl Pts',(4.00042123727896,18.9207316512905,-14.8048148488943));
#28821=CARTESIAN_POINT('Ctrl Pts',(3.94435406431171,18.3471385661789,-14.8326777457735));
#28822=CARTESIAN_POINT('Ctrl Pts',(4.08161076257883,17.9187745453667,-15.190051549908));
#28823=CARTESIAN_POINT('Ctrl Pts',(3.64551666599827,18.9604224970588,-14.9998401423731));
#28824=CARTESIAN_POINT('Ctrl Pts',(3.63144227309245,18.445112778749,-15.0057090520327));
#28825=CARTESIAN_POINT('Ctrl Pts',(3.7547644971397,18.0355093244708,-15.2941104791594));
#28826=CARTESIAN_POINT('Ctrl Pts',(2.92607962857322,18.9432173241542,-15.3261118849119));
#28827=CARTESIAN_POINT('Ctrl Pts',(2.96645048632596,18.5378314308947,-15.3082201989774));
#28828=CARTESIAN_POINT('Ctrl Pts',(3.0670243958767,18.1853707626654,-15.4855410702878));
#28829=CARTESIAN_POINT('Ctrl Pts',(2.55821923863863,18.8884652562898,-15.4610221971148));
#28830=CARTESIAN_POINT('Ctrl Pts',(2.61131053677853,18.53963094037,-15.442931777827));
#28831=CARTESIAN_POINT('Ctrl Pts',(2.702670137469,18.2245847172643,-15.5753398189059));
#28832=CARTESIAN_POINT('Ctrl Pts',(1.82891451879107,18.7188973096673,-15.6707363864532));
#28833=CARTESIAN_POINT('Ctrl Pts',(1.8915394318877,18.4751292210006,-15.655459830255));
#28834=CARTESIAN_POINT('Ctrl Pts',(1.96287487075161,18.2420370455397,-15.7200549068671));
#28835=CARTESIAN_POINT('Ctrl Pts',(1.46353131432253,18.6039976779082,-15.7477141653928));
#28836=CARTESIAN_POINT('Ctrl Pts',(1.5201038802911,18.4109076720057,-15.7376927883366));
#28837=CARTESIAN_POINT('Ctrl Pts',(1.5808347731626,18.2227697778871,-15.7776716140354));
#28838=CARTESIAN_POINT('Ctrl Pts',(0.729117484548387,18.3301937948796,-15.8501327863187));
#28839=CARTESIAN_POINT('Ctrl Pts',(0.765887787217641,18.2357095390798,-15.8471046364417));
#28840=CARTESIAN_POINT('Ctrl Pts',(0.800159021600452,18.1403975456869,-15.8549367139924));
#28841=CARTESIAN_POINT('Ctrl Pts',(0.361264579835011,18.1710404144994,-15.875));
#28842=CARTESIAN_POINT('Ctrl Pts',(0.379968202538298,18.1240305404275,-15.8749999999992));
#28843=CARTESIAN_POINT('Ctrl Pts',(0.3987363721605,18.0770350537944,-15.8749999999984));
#28844=CARTESIAN_POINT('Ctrl Pts',(4.96157966372969E-14,18.0000000000001,
-15.875));
#28845=CARTESIAN_POINT('Ctrl Pts',(4.96157966372969E-14,18.0000000000001,
-15.875));
#28846=CARTESIAN_POINT('Ctrl Pts',(4.96157966372969E-14,18.0000000000001,
-15.875));
#28847=CARTESIAN_POINT('Ctrl Pts',(4.26261338778694,18.0849267018157,-14.875));
#28848=CARTESIAN_POINT('Ctrl Pts',(3.95178714242438,18.188266342333,-15.0609320135528));
#28849=CARTESIAN_POINT('Ctrl Pts',(3.61923443569512,18.2429627164579,-15.2173202422925));
#28850=CARTESIAN_POINT('Ctrl Pts',(3.09548155756297,18.2860517458273,-15.411764578239));
#28851=CARTESIAN_POINT('Ctrl Pts',(2.91664062652119,18.2933512364512,-15.4698977560958));
#28852=CARTESIAN_POINT('Ctrl Pts',(2.55896263908662,18.2964774327613,-15.5720972662161));
#28853=CARTESIAN_POINT('Ctrl Pts',(2.37912173967026,18.2923841267789,-15.6165600378252));
#28854=CARTESIAN_POINT('Ctrl Pts',(1.83693290496417,18.2663432658698,-15.7326561330689));
#28855=CARTESIAN_POINT('Ctrl Pts',(1.47194228891703,18.2307806146048,-15.7871564550427));
#28856=CARTESIAN_POINT('Ctrl Pts',(0.735959210913914,18.1331323295489,-15.8585038606388));
#28857=CARTESIAN_POINT('Ctrl Pts',(0.364750325440251,18.0705479584007,-15.875));
#28858=CARTESIAN_POINT('Ctrl Pts',(5.55111512312578E-14,18.0000000000001,
-15.875));
#28859=CARTESIAN_POINT('Ctrl Pts',(2.65026635155863,16.5230910595128,-15.875));
#28860=CARTESIAN_POINT('Ctrl Pts',(3.93121151026238,17.4113360701453,-15.8749999999999));
#28861=CARTESIAN_POINT('Ctrl Pts',(4.67780976977134,17.9221915136298,-14.60813118344));
#28862=CARTESIAN_POINT('Ctrl Pts',(2.58982177486721,16.6081406311209,-15.875));
#28863=CARTESIAN_POINT('Ctrl Pts',(3.58403517899291,17.5024571546094,-15.875));
#28864=CARTESIAN_POINT('Ctrl Pts',(4.2564307312372,18.1092948426311,-14.8946688271178));
#28865=CARTESIAN_POINT('Ctrl Pts',(2.52003685548928,16.6804128457835,-15.875));
#28866=CARTESIAN_POINT('Ctrl Pts',(3.38378930551504,17.5440516972148,-15.875));
#28867=CARTESIAN_POINT('Ctrl Pts',(4.0035673119342,18.165009724916,-15.0260933099477));
#28868=CARTESIAN_POINT('Ctrl Pts',(2.40146991110847,16.7894204758253,-15.875));
#28869=CARTESIAN_POINT('Ctrl Pts',(3.10682864280578,17.6014533498092,-15.875));
#28870=CARTESIAN_POINT('Ctrl Pts',(3.65204402458872,18.2296067372696,-15.1932422733977));
#28871=CARTESIAN_POINT('Ctrl Pts',(2.35467715083744,16.8290896112474,-15.875));
#28872=CARTESIAN_POINT('Ctrl Pts',(3.01282991317325,17.6202437200566,-15.875));
#28873=CARTESIAN_POINT('Ctrl Pts',(3.5325569900976,18.2454983024018,-15.2442421923076));
#28874=CARTESIAN_POINT('Ctrl Pts',(2.21130584963083,16.9438587854015,-15.875));
#28875=CARTESIAN_POINT('Ctrl Pts',(2.74722464793244,17.6721885860779,-15.875));
#28876=CARTESIAN_POINT('Ctrl Pts',(3.1943476300972,18.2819216705679,-15.3791782895574));
#28877=CARTESIAN_POINT('Ctrl Pts',(2.11176395525861,17.014762601574,-15.875));
#28878=CARTESIAN_POINT('Ctrl Pts',(2.58832028065915,17.7015695819078,-15.875));
#28879=CARTESIAN_POINT('Ctrl Pts',(2.99607057193265,18.2908999426499,-15.4448482866377));
#28880=CARTESIAN_POINT('Ctrl Pts',(1.9075067361548,17.1492444573459,-15.875));
#28881=CARTESIAN_POINT('Ctrl Pts',(2.28363197198804,17.7549714543998,-15.875));
#28882=CARTESIAN_POINT('Ctrl Pts',(2.61932017223037,18.2973683425168,-15.5563761690608));
#28883=CARTESIAN_POINT('Ctrl Pts',(1.8027279134729,17.2127325814033,-15.875));
#28884=CARTESIAN_POINT('Ctrl Pts',(2.13794849055388,17.7789387893468,-15.8749999999995));
#28885=CARTESIAN_POINT('Ctrl Pts',(2.44212041430218,18.2940957945644,-15.6011724680293));
#28886=CARTESIAN_POINT('Ctrl Pts',(1.58907728513264,17.3339130080378,-15.875));
#28887=CARTESIAN_POINT('Ctrl Pts',(1.85327321501529,17.8227171794126,-15.8750000000004));
#28888=CARTESIAN_POINT('Ctrl Pts',(2.0996263813784,18.2799878268499,-15.6775823058619));
#28889=CARTESIAN_POINT('Ctrl Pts',(1.48001425485868,17.3916684380892,-15.875));
#28890=CARTESIAN_POINT('Ctrl Pts',(1.71380729714794,17.8426075850252,-15.8749999999998));
#28891=CARTESIAN_POINT('Ctrl Pts',(1.93430002680071,18.269009952329,-15.7090537912825));
#28892=CARTESIAN_POINT('Ctrl Pts',(1.14923719089035,17.5568620321583,-15.875));
#28893=CARTESIAN_POINT('Ctrl Pts',(1.30369857493354,17.8965847239176,-15.8750000000004));
#28894=CARTESIAN_POINT('Ctrl Pts',(1.45222631610486,18.2281607599578,-15.7886599080685));
#28895=CARTESIAN_POINT('Ctrl Pts',(0.923960370814538,17.6563936138833,-15.875));
#28896=CARTESIAN_POINT('Ctrl Pts',(1.03778172221532,17.9255569355278,-15.8749999999978));
#28897=CARTESIAN_POINT('Ctrl Pts',(1.14890106782412,18.1905780578685,-15.8223795985853));
#28898=CARTESIAN_POINT('Ctrl Pts',(0.466309887646269,17.8396525797121,-15.875));
#28899=CARTESIAN_POINT('Ctrl Pts',(0.514033028281665,17.9714545644638,-15.8750000000021));
#28900=CARTESIAN_POINT('Ctrl Pts',(0.560899725435248,18.1034285976806,-15.8657311564014));
#28901=CARTESIAN_POINT('Ctrl Pts',(0.233960073392275,17.9230862029257,-15.875));
#28902=CARTESIAN_POINT('Ctrl Pts',(0.255450344256121,17.9882387163098,-15.875));
#28903=CARTESIAN_POINT('Ctrl Pts',(0.276905092786154,18.0534927743003,-15.875));
#28904=CARTESIAN_POINT('Ctrl Pts',(6.56253264560329E-14,18.0000000000001,
-15.875));
#28905=CARTESIAN_POINT('Ctrl Pts',(6.56253264560329E-14,18.0000000000001,
-15.875));
#28906=CARTESIAN_POINT('Ctrl Pts',(6.56253264560329E-14,18.0000000000001,
-15.875));
#28907=CARTESIAN_POINT('Origin',(2.57755123502973,16.6150404676651,-12.875));
#28908=CARTESIAN_POINT('Ctrl Pts',(6.18681074697913,13.6646760949928,-15.875));
#28909=CARTESIAN_POINT('Ctrl Pts',(7.42417289637491,16.3976113139914,-15.875));
#28910=CARTESIAN_POINT('Ctrl Pts',(7.4241728963749,16.3976113139913,-12.8749999999999));
#28911=CARTESIAN_POINT('Ctrl Pts',(5.46924488951516,13.9895608039258,-15.875));
#28912=CARTESIAN_POINT('Ctrl Pts',(6.9364443429193,16.3422300389752,-15.8749999999987));
#28913=CARTESIAN_POINT('Ctrl Pts',(7.02429276766003,16.5786608069056,-13.1370575997094));
#28914=CARTESIAN_POINT('Ctrl Pts',(4.82362135451195,14.4304994470984,-15.875));
#28915=CARTESIAN_POINT('Ctrl Pts',(6.3369558752052,16.3976766216994,-15.875));
#28916=CARTESIAN_POINT('Ctrl Pts',(6.59593944537325,16.8198356081028,-13.4464657347114));
#28917=CARTESIAN_POINT('Ctrl Pts',(3.62953325538149,15.4524280214079,-15.875));
#28918=CARTESIAN_POINT('Ctrl Pts',(5.01707693139717,16.7889673744352,-15.875));
#28919=CARTESIAN_POINT('Ctrl Pts',(5.57070135292839,17.4021716501979,-14.1426663720984));
#28920=CARTESIAN_POINT('Ctrl Pts',(3.09339544139825,16.0236820718619,-15.875));
#28921=CARTESIAN_POINT('Ctrl Pts',(4.32161737669038,17.1014577313411,-15.875));
#28922=CARTESIAN_POINT('Ctrl Pts',(4.98189659820059,17.7388522671779,-14.5233265662417));
#28923=CARTESIAN_POINT('Ctrl Pts',(2.57755123502973,16.615040467665,-15.875));
#28924=CARTESIAN_POINT('Ctrl Pts',(3.58858852668408,17.4969722081554,-15.875));
#28925=CARTESIAN_POINT('Ctrl Pts',(4.26261338778696,18.0849267018156,-14.8749999999999));
#28926=CARTESIAN_POINT('Ctrl Pts',(-2.57755123502973,16.6150404676652,-15.875));
#28927=CARTESIAN_POINT('Ctrl Pts',(-3.58858852668405,17.4969722081555,-15.875));
#28928=CARTESIAN_POINT('Ctrl Pts',(-4.26261338778693,18.0849267018157,-14.875));
#28929=CARTESIAN_POINT('Ctrl Pts',(-3.09288471114456,16.0242675681528,-15.875));
#28930=CARTESIAN_POINT('Ctrl Pts',(-4.32097890338961,17.1018022275832,-15.875));
#28931=CARTESIAN_POINT('Ctrl Pts',(-4.98122339764458,17.7391761695861,-14.5236557087854));
#28932=CARTESIAN_POINT('Ctrl Pts',(-3.627647853051,15.4550005401893,-15.875));
#28933=CARTESIAN_POINT('Ctrl Pts',(-5.01362902801974,16.7908754694181,-15.875));
#28934=CARTESIAN_POINT('Ctrl Pts',(-5.56799291687747,17.403710991418,-14.1443060928063));
#28935=CARTESIAN_POINT('Ctrl Pts',(-4.51455185470875,14.6945381515796,-15.875));
#28936=CARTESIAN_POINT('Ctrl Pts',(-5.97317586756606,16.5050589588183,-15.875));
#28937=CARTESIAN_POINT('Ctrl Pts',(-6.33110821894754,16.9702594914345,-13.6264004799583));
#28938=CARTESIAN_POINT('Ctrl Pts',(-4.82417650767969,14.4564823289508,-15.875));
#28939=CARTESIAN_POINT('Ctrl Pts',(-6.28922934917424,16.4389856109726,-15.875));
#28940=CARTESIAN_POINT('Ctrl Pts',(-6.56619762783053,16.8368211352426,-13.4613493294144));
#28941=CARTESIAN_POINT('Ctrl Pts',(-5.48132765779044,14.0221782762144,-15.875));
#28942=CARTESIAN_POINT('Ctrl Pts',(-6.89238296370854,16.3693310552367,-15.875));
#28943=CARTESIAN_POINT('Ctrl Pts',(-7.01312239354118,16.5954930631039,-13.1508837135674));
#28944=CARTESIAN_POINT('Ctrl Pts',(-5.827547276862,13.8273360156432,-15.875));
#28945=CARTESIAN_POINT('Ctrl Pts',(-7.17519783431907,16.3693403474512,-15.875000000002));
#28946=CARTESIAN_POINT('Ctrl Pts',(-7.22390466722361,16.4882846401484,-13.0062438591931));
#28947=CARTESIAN_POINT('Ctrl Pts',(-6.18681074697824,13.6646760949932,-15.875));
#28948=CARTESIAN_POINT('Ctrl Pts',(-7.42417289637423,16.3976113139912,-15.875));
#28949=CARTESIAN_POINT('Ctrl Pts',(-7.42417289637437,16.3976113139916,-12.8750000000003));
#28950=CARTESIAN_POINT('Origin',(-2.57755123502973,16.6150404676652,-12.875));
#28951=CARTESIAN_POINT('Ctrl Pts',(7.10299919046342E-14,18.0000000000001,
-15.875));
#28952=CARTESIAN_POINT('Ctrl Pts',(7.10299919046342E-14,18.0000000000001,
-15.875));
#28953=CARTESIAN_POINT('Ctrl Pts',(7.10299919046342E-14,18.0000000000001,
-15.875));
#28954=CARTESIAN_POINT('Ctrl Pts',(-0.234069005549895,17.9230507329212,
-15.875));
#28955=CARTESIAN_POINT('Ctrl Pts',(-0.255572484264496,17.9883108104968,
-15.875));
#28956=CARTESIAN_POINT('Ctrl Pts',(-0.277021629265281,18.0535866911956,
-15.875));
#28957=CARTESIAN_POINT('Ctrl Pts',(-0.465540714391679,17.8399080016609,
-15.875));
#28958=CARTESIAN_POINT('Ctrl Pts',(-0.513189867278885,17.9714965813304,
-15.8750000000013));
#28959=CARTESIAN_POINT('Ctrl Pts',(-0.559992022757088,18.1032500480137,
-15.865732501886));
#28960=CARTESIAN_POINT('Ctrl Pts',(-0.920922503725983,17.6576622237466,
-15.875));
#28961=CARTESIAN_POINT('Ctrl Pts',(-1.03425506051337,17.9258961394952,-15.8749999999987));
#28962=CARTESIAN_POINT('Ctrl Pts',(-1.14491687502606,18.1900283969107,-15.8227387473914));
#28963=CARTESIAN_POINT('Ctrl Pts',(-1.14500232012262,17.5587569237231,-15.875));
#28964=CARTESIAN_POINT('Ctrl Pts',(-1.29867014733387,17.8971439307737,-15.8750000000008));
#28965=CARTESIAN_POINT('Ctrl Pts',(-1.44648584682184,18.2274660352735,-15.7893261010449));
#28966=CARTESIAN_POINT('Ctrl Pts',(-1.47389755518,17.3948291236,-15.875));
#28967=CARTESIAN_POINT('Ctrl Pts',(-1.70607551178078,17.8436724534546,-15.8749999999996));
#28968=CARTESIAN_POINT('Ctrl Pts',(-1.92517570374991,18.2683328929667,-15.7106973352853));
#28969=CARTESIAN_POINT('Ctrl Pts',(-1.58231605112504,17.3375717912511,-15.875));
#28970=CARTESIAN_POINT('Ctrl Pts',(-1.84452054067363,17.8239944625641,-15.875));
#28971=CARTESIAN_POINT('Ctrl Pts',(-2.08919765818595,18.2793742064832,-15.6796758611809));
#28972=CARTESIAN_POINT('Ctrl Pts',(-1.79616610743275,17.2166198358638,-15.875));
#28973=CARTESIAN_POINT('Ctrl Pts',(-2.12895470680322,17.7803825956827,-15.875));
#28974=CARTESIAN_POINT('Ctrl Pts',(-2.43121242086649,18.2938125595251,-15.6038274824088));
#28975=CARTESIAN_POINT('Ctrl Pts',(-1.90161128728044,17.1529545648422,-15.875));
#28976=CARTESIAN_POINT('Ctrl Pts',(-2.27519611057993,17.7563986700479,-15.875));
#28977=CARTESIAN_POINT('Ctrl Pts',(-2.60895323727161,18.2973410269971,-15.5592038314364));
#28978=CARTESIAN_POINT('Ctrl Pts',(-2.10852690803343,17.0170578688654,-15.875));
#28979=CARTESIAN_POINT('Ctrl Pts',(-2.58317026964648,17.7025162702681,-15.875));
#28980=CARTESIAN_POINT('Ctrl Pts',(-2.98960933272182,18.2911991025238,-15.4469955360255));
#28981=CARTESIAN_POINT('Ctrl Pts',(-2.20977219872288,16.9450430793437,-15.875));
#28982=CARTESIAN_POINT('Ctrl Pts',(-2.74453268668338,17.6727031367294,-15.875));
#28983=CARTESIAN_POINT('Ctrl Pts',(-3.19091502304556,18.2822213950292,-15.3804805124035));
#28984=CARTESIAN_POINT('Ctrl Pts',(-2.35442817124508,16.8293103914149,-15.875));
#28985=CARTESIAN_POINT('Ctrl Pts',(-3.01230037937074,17.6203479307052,-15.875));
#28986=CARTESIAN_POINT('Ctrl Pts',(-3.53187268765323,18.2455993729309,-15.2445526648722));
#28987=CARTESIAN_POINT('Ctrl Pts',(-2.40151582425997,16.7893870879841,-15.875));
#28988=CARTESIAN_POINT('Ctrl Pts',(-3.106895543949,17.6014376117974,-15.875));
#28989=CARTESIAN_POINT('Ctrl Pts',(-3.65212401943686,18.2296036955527,-15.1932231473742));
#28990=CARTESIAN_POINT('Ctrl Pts',(-2.5194290407753,16.6809575628544,-15.875));
#28991=CARTESIAN_POINT('Ctrl Pts',(-3.38240321244847,17.5443315105624,-15.875));
#28992=CARTESIAN_POINT('Ctrl Pts',(-4.0018443914251,18.1652942771662,-15.0268910373232));
#28993=CARTESIAN_POINT('Ctrl Pts',(-2.58809131240417,16.6098149497214,-15.875));
#28994=CARTESIAN_POINT('Ctrl Pts',(-3.5795504098364,17.5033224532898,-15.875));
#28995=CARTESIAN_POINT('Ctrl Pts',(-4.25085054079885,18.1101703713992,-14.8973061650154));
#28996=CARTESIAN_POINT('Ctrl Pts',(-2.64710716057363,16.5274299671713,-15.875));
#28997=CARTESIAN_POINT('Ctrl Pts',(-3.91380212598874,17.4158477301436,-15.875));
#28998=CARTESIAN_POINT('Ctrl Pts',(-4.65725862181919,17.9310735147891,-14.6219520331606));
#28999=CARTESIAN_POINT('Ctrl Pts',(1.34330150810747E-13,18.,-3.25260651745651E-15));
#29000=CARTESIAN_POINT('Ctrl Pts',(1.34330150810747E-13,18.,-3.25260651745651E-15));
#29001=CARTESIAN_POINT('Ctrl Pts',(1.34330150810747E-13,18.,-3.25260651745651E-15));
#29002=CARTESIAN_POINT('Ctrl Pts',(0.234125392939614,17.9230321957875,-3.90312782094782E-15));
#29003=CARTESIAN_POINT('Ctrl Pts',(0.255636569916122,17.9883077450276,-5.57090702034659E-15));
#29004=CARTESIAN_POINT('Ctrl Pts',(0.277092073072303,18.0536000698534,-7.23849759038514E-15));
#29005=CARTESIAN_POINT('Ctrl Pts',(0.466044116165369,17.8397456189194,-3.90312782094782E-15));
#29006=CARTESIAN_POINT('Ctrl Pts',(0.513738375516134,17.9714716147092,2.5996297196232E-12));
#29007=CARTESIAN_POINT('Ctrl Pts',(0.560578310461167,18.1033685423708,-0.00926178509230557));
#29008=CARTESIAN_POINT('Ctrl Pts',(0.923258246822673,17.6566881249403,-3.90312782094782E-15));
#29009=CARTESIAN_POINT('Ctrl Pts',(1.03696511564348,17.9256348627915,-2.63383661051795E-12));
#29010=CARTESIAN_POINT('Ctrl Pts',(1.14797712170856,18.1904491877953,-0.0525350981222591));
#29011=CARTESIAN_POINT('Ctrl Pts',(1.14901068589157,17.5569249384112,-3.90312782094782E-15));
#29012=CARTESIAN_POINT('Ctrl Pts',(1.3034614298748,17.8965907426942,-7.42089362459187E-13));
#29013=CARTESIAN_POINT('Ctrl Pts',(1.45199329102125,18.2280903008762,-0.0863653390068735));
#29014=CARTESIAN_POINT('Ctrl Pts',(1.47823538432377,17.3925817155132,-3.90312782094782E-15));
#29015=CARTESIAN_POINT('Ctrl Pts',(1.71156276414173,17.8429116909266,3.72586727994298E-13));
#29016=CARTESIAN_POINT('Ctrl Pts',(1.93165601447728,18.2688045577474,-0.16547617335809));
#29017=CARTESIAN_POINT('Ctrl Pts',(1.5865002670268,17.3352987442417,-3.90312782094782E-15));
#29018=CARTESIAN_POINT('Ctrl Pts',(1.84994552041935,17.8231970718718,7.48227181606773E-14));
#29019=CARTESIAN_POINT('Ctrl Pts',(2.09567016562423,18.2797417545793,-0.196634467066437));
#29020=CARTESIAN_POINT('Ctrl Pts',(1.79944928043518,17.2146660494541,-3.90312782094782E-15));
#29021=CARTESIAN_POINT('Ctrl Pts',(2.13346302307632,17.7796530524275,-8.44427400896034E-14));
#29022=CARTESIAN_POINT('Ctrl Pts',(2.43668826790097,18.2939422278445,-0.272515027710232));
#29023=CARTESIAN_POINT('Ctrl Pts',(1.90414773824699,17.151340599891,-3.90312782094782E-15));
#29024=CARTESIAN_POINT('Ctrl Pts',(2.27885177250061,17.7557724864729,8.90502107893631E-14));
#29025=CARTESIAN_POINT('Ctrl Pts',(2.61346406100076,18.2973270865418,-0.317051368781859));
#29026=CARTESIAN_POINT('Ctrl Pts',(2.1088743828907,17.0167770117627,-3.90312782094782E-15));
#29027=CARTESIAN_POINT('Ctrl Pts',(2.58377885264389,17.7023930210976,-9.69193503961864E-14));
#29028=CARTESIAN_POINT('Ctrl Pts',(2.99040325834679,18.2911221026525,-0.428311953949879));
#29029=CARTESIAN_POINT('Ctrl Pts',(2.20896418655429,16.9456432686019,-3.90312782094782E-15));
#29030=CARTESIAN_POINT('Ctrl Pts',(2.74317790194251,17.6729570612561,2.28883521929507E-14));
#29031=CARTESIAN_POINT('Ctrl Pts',(3.18920946464565,18.2823326069824,-0.493912463383087));
#29032=CARTESIAN_POINT('Ctrl Pts',(2.3537482518898,16.8298772373725,-3.90312782094782E-15));
#29033=CARTESIAN_POINT('Ctrl Pts',(3.01096091470094,17.6206124704897,-1.71623730517786E-14));
#29034=CARTESIAN_POINT('Ctrl Pts',(3.5301688979625,18.2458140896114,-0.629729813065811));
#29035=CARTESIAN_POINT('Ctrl Pts',(2.40124097545901,16.7896357735171,-3.90312782094782E-15));
#29036=CARTESIAN_POINT('Ctrl Pts',(3.10627843143028,17.601562552945,-1.66557843234476E-14));
#29037=CARTESIAN_POINT('Ctrl Pts',(3.65133078641054,18.2297390382189,-0.681405276743203));
#29038=CARTESIAN_POINT('Ctrl Pts',(2.5189927470668,16.681365157594,-3.90312782094782E-15));
#29039=CARTESIAN_POINT('Ctrl Pts',(3.38133850977177,17.5445513739635,1.81195115538009E-14));
#29040=CARTESIAN_POINT('Ctrl Pts',(4.00051020852894,18.1655490559811,-0.847460814619883));
#29041=CARTESIAN_POINT('Ctrl Pts',(2.58698239764016,16.6108854489588,-3.90312782094782E-15));
#29042=CARTESIAN_POINT('Ctrl Pts',(3.57666092871365,17.5038821817581,-9.64497019840983E-14));
#29043=CARTESIAN_POINT('Ctrl Pts',(4.2472541605191,18.1107431001,-0.975990516500565));
#29044=CARTESIAN_POINT('Ctrl Pts',(2.64500586200195,16.5302897988031,-3.90312782094782E-15));
#29045=CARTESIAN_POINT('Ctrl Pts',(3.90245585433798,17.4187779420453,1.36808593330039E-13));
#29046=CARTESIAN_POINT('Ctrl Pts',(4.64383425604972,17.9368198526809,-1.24406142456628));
#29047=CARTESIAN_POINT('Origin',(2.57755123502973,16.6150404676649,-3.));
#29048=CARTESIAN_POINT('Ctrl Pts',(2.57755123502973,16.6150404676649,-3.90312782094782E-15));
#29049=CARTESIAN_POINT('Ctrl Pts',(3.58858852668408,17.4969722081553,-4.11996825544492E-15));
#29050=CARTESIAN_POINT('Ctrl Pts',(4.26261338778696,18.0849267018155,-1.00000000000006));
#29051=CARTESIAN_POINT('Ctrl Pts',(3.09288471119035,16.0242675681923,-3.90312782094782E-15));
#29052=CARTESIAN_POINT('Ctrl Pts',(4.32097890344208,17.1018022276782,8.76728492794768E-13));
#29053=CARTESIAN_POINT('Ctrl Pts',(4.98122339765377,17.7391761696867,-1.35134429129639));
#29054=CARTESIAN_POINT('Ctrl Pts',(3.62764785305072,15.4550005401872,-3.90312782094782E-15));
#29055=CARTESIAN_POINT('Ctrl Pts',(5.01362902801955,16.7908754694178,-3.67888638612552E-13));
#29056=CARTESIAN_POINT('Ctrl Pts',(5.56799291687799,17.4037109914178,-1.73069390719434));
#29057=CARTESIAN_POINT('Ctrl Pts',(4.51455185471047,14.6945381515792,-3.90312782094782E-15));
#29058=CARTESIAN_POINT('Ctrl Pts',(5.9731758675679,16.5050589588179,1.90369720475917E-13));
#29059=CARTESIAN_POINT('Ctrl Pts',(6.33110821894858,16.9702594914338,-2.2485995200423));
#29060=CARTESIAN_POINT('Ctrl Pts',(4.82417650768106,14.4564823289491,-3.90312782094782E-15));
#29061=CARTESIAN_POINT('Ctrl Pts',(6.2892293491753,16.4389856109718,1.00596761688566E-13));
#29062=CARTESIAN_POINT('Ctrl Pts',(6.56619762783129,16.8368211352422,-2.41365067058626));
#29063=CARTESIAN_POINT('Ctrl Pts',(5.48132765779251,14.0221782762138,-3.90312782094782E-15));
#29064=CARTESIAN_POINT('Ctrl Pts',(6.89238296371062,16.3693310552372,-1.130184358169E-13));
#29065=CARTESIAN_POINT('Ctrl Pts',(7.01312239354269,16.595493063103,-2.72411628643354));
#29066=CARTESIAN_POINT('Ctrl Pts',(5.82754727684479,13.8273360155938,-3.90312782094782E-15));
#29067=CARTESIAN_POINT('Ctrl Pts',(7.17519783432794,16.3693403473953,-1.82423844731643E-12));
#29068=CARTESIAN_POINT('Ctrl Pts',(7.22390466723139,16.4882846401449,-2.868756140798));
#29069=CARTESIAN_POINT('Ctrl Pts',(6.18681074697836,13.6646760949931,-3.90312782094782E-15));
#29070=CARTESIAN_POINT('Ctrl Pts',(7.42417289637432,16.3976113139913,-3.90312782096724E-15));
#29071=CARTESIAN_POINT('Ctrl Pts',(7.42417289637442,16.3976113139915,-2.99999999999976));
#29072=CARTESIAN_POINT('Ctrl Pts',(-6.18681074697897,13.6646760949927,-4.33680868994202E-15));
#29073=CARTESIAN_POINT('Ctrl Pts',(-7.42417289637478,16.3976113139913,-4.33680868994226E-15));
#29074=CARTESIAN_POINT('Ctrl Pts',(-7.42417289637476,16.3976113139913,-3.00000000000003));
#29075=CARTESIAN_POINT('Ctrl Pts',(-5.46924488956975,13.9895608040479,-4.33680868994202E-15));
#29076=CARTESIAN_POINT('Ctrl Pts',(-6.93644434272296,16.3422300407555,6.3950190944217E-13));
#29077=CARTESIAN_POINT('Ctrl Pts',(-7.02429276683661,16.5786608072783,-2.73794240179331));
#29078=CARTESIAN_POINT('Ctrl Pts',(-4.82362135451254,14.4304994470984,-3.90312782094782E-15));
#29079=CARTESIAN_POINT('Ctrl Pts',(-6.33695587520574,16.3976766216994,-2.26478507750015E-13));
#29080=CARTESIAN_POINT('Ctrl Pts',(-6.59593944537465,16.8198356081016,-2.42853426528885));
#29081=CARTESIAN_POINT('Ctrl Pts',(-3.62953325538071,15.4524280214079,-3.90312782094782E-15));
#29082=CARTESIAN_POINT('Ctrl Pts',(-5.01707693139635,16.7889673744352,2.00368435798586E-13));
#29083=CARTESIAN_POINT('Ctrl Pts',(-5.57070135292674,17.4021716501991,-1.73233362790125));
#29084=CARTESIAN_POINT('Ctrl Pts',(-3.0933954413352,16.0236820718031,-3.90312782094782E-15));
#29085=CARTESIAN_POINT('Ctrl Pts',(-4.32161737629064,17.101457730593,-7.08979370270738E-13));
#29086=CARTESIAN_POINT('Ctrl Pts',(-4.98189659816054,17.7388522667007,-1.35167343337454));
#29087=CARTESIAN_POINT('Ctrl Pts',(-2.57755123502756,16.6150404676675,-3.90312782094782E-15));
#29088=CARTESIAN_POINT('Ctrl Pts',(-3.58858852668275,17.4969722081568,-3.68628738645072E-15));
#29089=CARTESIAN_POINT('Ctrl Pts',(-4.2626133877862,18.0849267018164,-1.00000000000002));
#29090=CARTESIAN_POINT('Origin',(-2.57755123502967,16.6150404676651,-3.));
#29091=CARTESIAN_POINT('Ctrl Pts',(-2.65026635075671,16.5230910607405,-3.90312782094782E-15));
#29092=CARTESIAN_POINT('Ctrl Pts',(-3.93121150527454,17.4113360715034,-2.40519271556319E-14));
#29093=CARTESIAN_POINT('Ctrl Pts',(-4.67780976387663,17.9221915162604,-1.26686881256096));
#29094=CARTESIAN_POINT('Ctrl Pts',(-2.58982177419273,16.6081406317741,-3.90312782094782E-15));
#29095=CARTESIAN_POINT('Ctrl Pts',(-3.58403517709281,17.502457154976,-7.58581112797788E-16));
#29096=CARTESIAN_POINT('Ctrl Pts',(-4.25643072887683,18.1092948431411,-0.98033117164757));
#29097=CARTESIAN_POINT('Ctrl Pts',(-2.520036855148,16.6804128460974,-3.90312782094782E-15));
#29098=CARTESIAN_POINT('Ctrl Pts',(-3.3837893047036,17.5440516973813,6.73959394317873E-15));
#29099=CARTESIAN_POINT('Ctrl Pts',(-4.0035673109207,18.1650097251003,-0.848906689568997));
#29100=CARTESIAN_POINT('Ctrl Pts',(-2.4014699111082,16.7894204758251,-3.90312782094782E-15));
#29101=CARTESIAN_POINT('Ctrl Pts',(-3.10682864280438,17.6014533498079,-1.0760287253188E-14));
#29102=CARTESIAN_POINT('Ctrl Pts',(-3.6520440245868,18.2296067372679,-0.681757726600342));
#29103=CARTESIAN_POINT('Ctrl Pts',(-2.35467715083726,16.8290896112472,-3.90312782094782E-15));
#29104=CARTESIAN_POINT('Ctrl Pts',(-3.01282991317201,17.6202437200552,9.82896428929409E-15));
#29105=CARTESIAN_POINT('Ctrl Pts',(-3.53255699009597,18.2454983024002,-0.630757807690744));
#29106=CARTESIAN_POINT('Ctrl Pts',(-2.21130584963072,16.9438587854014,-3.90312782094782E-15));
#29107=CARTESIAN_POINT('Ctrl Pts',(-2.74722464793154,17.672188586077,-2.97020675421629E-14));
#29108=CARTESIAN_POINT('Ctrl Pts',(-3.19434763009571,18.2819216705659,-0.495821710441106));
#29109=CARTESIAN_POINT('Ctrl Pts',(-2.11176395525848,17.0147626015738,-3.90312782094782E-15));
#29110=CARTESIAN_POINT('Ctrl Pts',(-2.58832028065808,17.7015695819063,-7.00728626402298E-14));
#29111=CARTESIAN_POINT('Ctrl Pts',(-2.99607057193134,18.2908999426481,-0.430151713361074));
#29112=CARTESIAN_POINT('Ctrl Pts',(-1.90750673615457,17.1492444573458,-3.90312782094782E-15));
#29113=CARTESIAN_POINT('Ctrl Pts',(-2.28363197198743,17.7549714543992,6.25362877129781E-14));
#29114=CARTESIAN_POINT('Ctrl Pts',(-2.61932017222916,18.2973683425155,-0.318623830938357));
#29115=CARTESIAN_POINT('Ctrl Pts',(-1.8027279134725,17.2127325814031,-3.90312782094782E-15));
#29116=CARTESIAN_POINT('Ctrl Pts',(-2.13794849055309,17.7789387893463,-1.6446554081392E-13));
#29117=CARTESIAN_POINT('Ctrl Pts',(-2.44212041430075,18.2940957945633,-0.273827531969986));
#29118=CARTESIAN_POINT('Ctrl Pts',(-1.58907728513264,17.3339130080377,-3.90312782094782E-15));
#29119=CARTESIAN_POINT('Ctrl Pts',(-1.85327321501476,17.8227171794114,1.55159105695241E-13));
#29120=CARTESIAN_POINT('Ctrl Pts',(-2.09962638137778,18.2799878268482,-0.197417694137515));
#29121=CARTESIAN_POINT('Ctrl Pts',(-1.48001425485894,17.3916684380896,-3.90312782094782E-15));
#29122=CARTESIAN_POINT('Ctrl Pts',(-1.71380729714811,17.8426075850251,-1.06713969348454E-13));
#29123=CARTESIAN_POINT('Ctrl Pts',(-1.93430002680081,18.2690099523279,-0.165946208717278));
#29124=CARTESIAN_POINT('Ctrl Pts',(-1.14923719088923,17.5568620321569,-3.90312782094782E-15));
#29125=CARTESIAN_POINT('Ctrl Pts',(-1.30369857493165,17.8965847239158,2.13313069839087E-13));
#29126=CARTESIAN_POINT('Ctrl Pts',(-1.45222631610225,18.2281607599565,-0.0863400919308878));
#29127=CARTESIAN_POINT('Ctrl Pts',(-0.923960370814179,17.6563936138833,
-3.90312782094782E-15));
#29128=CARTESIAN_POINT('Ctrl Pts',(-1.03778172221478,17.9255569355276,-4.02138859125459E-12));
#29129=CARTESIAN_POINT('Ctrl Pts',(-1.14890106782272,18.1905780578673,-0.0526204014144626));
#29130=CARTESIAN_POINT('Ctrl Pts',(-0.466309887646034,17.8396525797112,
-3.90312782094782E-15));
#29131=CARTESIAN_POINT('Ctrl Pts',(-0.514033028281307,17.971454564463,3.99686269630224E-12));
#29132=CARTESIAN_POINT('Ctrl Pts',(-0.560899725435443,18.1034285976806,
-0.0092688435986574));
#29133=CARTESIAN_POINT('Ctrl Pts',(-0.233960073391672,17.9230862029248,
-3.90312782094782E-15));
#29134=CARTESIAN_POINT('Ctrl Pts',(-0.255450344254625,17.9882387163068,
-4.24790311669457E-15));
#29135=CARTESIAN_POINT('Ctrl Pts',(-0.276905092784516,18.0534927742982,
-4.59293432271516E-15));
#29136=CARTESIAN_POINT('Ctrl Pts',(1.00908127238944E-13,18.,-3.25260651745651E-15));
#29137=CARTESIAN_POINT('Ctrl Pts',(1.00908127238944E-13,18.,-3.25260651745651E-15));
#29138=CARTESIAN_POINT('Ctrl Pts',(1.00908127238944E-13,18.,-3.25260651745651E-15));
#29139=CARTESIAN_POINT('',(0.,0.,0.));
#29140=CARTESIAN_POINT('Origin',(-3.44169137633799E-14,15.9887500034686,
-8.78459658321108E-14));
#29141=CARTESIAN_POINT('',(6.56268467749993,2.3362500034686,-1.60601788046217E-13));
#29142=CARTESIAN_POINT('',(6.56268467750004,1.7012500034686,-1.65295427412214E-13));
#29143=CARTESIAN_POINT('',(6.56268467749992,15.9887500034686,-1.19377083354552E-13));
#29144=CARTESIAN_POINT('',(-3.17934379362961,0.,-5.74113257277709));
#29145=CARTESIAN_POINT('Ctrl Pts',(6.56268467750004,1.7012500034686,0.));
#29146=CARTESIAN_POINT('Ctrl Pts',(6.56268467750014,1.57425000346862,2.13234551188562));
#29147=CARTESIAN_POINT('Ctrl Pts',(5.30932343282148,1.44725000346863,3.85744926888032));
#29148=CARTESIAN_POINT('Ctrl Pts',(4.05596218814318,1.32025000346859,5.58255302587488));
#29149=CARTESIAN_POINT('Ctrl Pts',(2.0279810940716,1.19325000346859,6.2414840269267));
#29150=CARTESIAN_POINT('Ctrl Pts',(0.,1.06625000346873,6.90041502797853));
#29151=CARTESIAN_POINT('Ctrl Pts',(-2.0279810940716,0.939250003468617,6.2414840269267));
#29152=CARTESIAN_POINT('Ctrl Pts',(-4.05596218814312,0.81225000346864,5.58255302587488));
#29153=CARTESIAN_POINT('Ctrl Pts',(-5.30932343282148,0.685250003468529,
3.85744926888032));
#29154=CARTESIAN_POINT('Ctrl Pts',(-6.56268467749997,0.558250003468608,
2.13234551188562));
#29155=CARTESIAN_POINT('Ctrl Pts',(-6.5626846775001,0.431250003468608,0.));
#29156=CARTESIAN_POINT('Ctrl Pts',(-6.56268467750003,0.304250003468635,
-2.13234551188562));
#29157=CARTESIAN_POINT('Ctrl Pts',(-5.30932343282153,0.177250003468632,
-3.85744926888032));
#29158=CARTESIAN_POINT('Ctrl Pts',(-4.45333360667123,0.0905146680793477,
-5.03561818970082));
#29159=CARTESIAN_POINT('Ctrl Pts',(-3.17934379362961,0.,-5.74113257277708));
#29160=CARTESIAN_POINT('',(5.75296004380515,0.,-3.15789184594317));
#29161=CARTESIAN_POINT('Origin',(-3.4416913763381E-14,0.,-3.24209513641145E-13));
#29162=CARTESIAN_POINT('Ctrl Pts',(6.56268467749993,2.3362500034686,0.));
#29163=CARTESIAN_POINT('Ctrl Pts',(6.56268467750003,2.20925000346864,2.13234551188562));
#29164=CARTESIAN_POINT('Ctrl Pts',(5.30932343282159,2.08225000346862,3.85744926888032));
#29165=CARTESIAN_POINT('Ctrl Pts',(4.05596218814324,1.95525000346861,5.58255302587488));
#29166=CARTESIAN_POINT('Ctrl Pts',(2.02798109407148,1.82825000346865,6.2414840269267));
#29167=CARTESIAN_POINT('Ctrl Pts',(1.1673575708729E-13,1.70125000346858,
6.90041502797853));
#29168=CARTESIAN_POINT('Ctrl Pts',(-2.02798109407148,1.57425000346872,6.2414840269267));
#29169=CARTESIAN_POINT('Ctrl Pts',(-4.05596218814306,1.44725000346872,5.58255302587488));
#29170=CARTESIAN_POINT('Ctrl Pts',(-5.30932343282159,1.32025000346858,3.85744926888032));
#29171=CARTESIAN_POINT('Ctrl Pts',(-6.56268467750003,1.19325000346869,2.13234551188562));
#29172=CARTESIAN_POINT('Ctrl Pts',(-6.56268467749999,1.06625000346861,0.));
#29173=CARTESIAN_POINT('Ctrl Pts',(-6.56268467749997,0.939250003468656,
-2.13234551188562));
#29174=CARTESIAN_POINT('Ctrl Pts',(-5.30932343282164,0.812250003468629,
-3.85744926888032));
#29175=CARTESIAN_POINT('Ctrl Pts',(-4.05596218814312,0.685250003468624,
-5.58255302587488));
#29176=CARTESIAN_POINT('Ctrl Pts',(-2.02798109407154,0.558250003468708,
-6.2414840269267));
#29177=CARTESIAN_POINT('Ctrl Pts',(0.,0.431250003468709,-6.90041502797853));
#29178=CARTESIAN_POINT('Ctrl Pts',(2.02798109407154,0.30425000346862,-6.2414840269267));
#29179=CARTESIAN_POINT('Ctrl Pts',(4.05596218814306,0.177250003468736,-5.58255302587488));
#29180=CARTESIAN_POINT('Ctrl Pts',(5.30932343282159,0.0502500034685882,
-3.85744926888032));
#29181=CARTESIAN_POINT('Ctrl Pts',(5.55326106788226,0.0255324052627934,
-3.52169791826031));
#29182=CARTESIAN_POINT('Ctrl Pts',(5.75296004380515,0.,-3.15789184594317));
#29183=CARTESIAN_POINT('Origin',(-3.44169137633799E-14,15.9887500034686,
-8.78459658321108E-14));
#29184=CARTESIAN_POINT('',(6.56268467749999,4.87625000346864,-1.41827230582227E-13));
#29185=CARTESIAN_POINT('',(6.5626846775001,4.24125000346864,-1.46520869948225E-13));
#29186=CARTESIAN_POINT('',(6.56268467749992,15.9887500034686,-1.19377083354552E-13));
#29187=CARTESIAN_POINT('Ctrl Pts',(6.5626846775001,4.24125000346864,0.));
#29188=CARTESIAN_POINT('Ctrl Pts',(6.56268467750003,4.1142500034687,2.13234551188562));
#29189=CARTESIAN_POINT('Ctrl Pts',(5.30932343282148,3.98725000346861,3.85744926888032));
#29190=CARTESIAN_POINT('Ctrl Pts',(4.05596218814318,3.86025000346873,5.58255302587488));
#29191=CARTESIAN_POINT('Ctrl Pts',(2.0279810940716,3.73325000346858,6.2414840269267));
#29192=CARTESIAN_POINT('Ctrl Pts',(0.,3.60625000346864,6.90041502797853));
#29193=CARTESIAN_POINT('Ctrl Pts',(-2.0279810940716,3.4792500034686,6.2414840269267));
#29194=CARTESIAN_POINT('Ctrl Pts',(-4.05596218814312,3.35225000346861,5.58255302587488));
#29195=CARTESIAN_POINT('Ctrl Pts',(-5.30932343282159,3.22525000346852,3.85744926888032));
#29196=CARTESIAN_POINT('Ctrl Pts',(-6.56268467749991,3.09825000346869,2.13234551188562));
#29197=CARTESIAN_POINT('Ctrl Pts',(-6.5626846775001,2.9712500034686,0.));
#29198=CARTESIAN_POINT('Ctrl Pts',(-6.56268467750003,2.8442500034686,-2.13234551188562));
#29199=CARTESIAN_POINT('Ctrl Pts',(-5.30932343282148,2.71725000346862,-3.85744926888032));
#29200=CARTESIAN_POINT('Ctrl Pts',(-4.05596218814306,2.59025000346863,-5.58255302587488));
#29201=CARTESIAN_POINT('Ctrl Pts',(-2.02798109407165,2.46325000346864,-6.2414840269267));
#29202=CARTESIAN_POINT('Ctrl Pts',(0.,2.3362500034686,-6.90041502797853));
#29203=CARTESIAN_POINT('Ctrl Pts',(2.02798109407165,2.20925000346861,-6.2414840269267));
#29204=CARTESIAN_POINT('Ctrl Pts',(4.05596218814312,2.08225000346851,-5.58255302587488));
#29205=CARTESIAN_POINT('Ctrl Pts',(5.30932343282148,1.95525000346858,-3.85744926888032));
#29206=CARTESIAN_POINT('Ctrl Pts',(6.56268467749997,1.82825000346865,-2.13234551188562));
#29207=CARTESIAN_POINT('Ctrl Pts',(6.56268467750004,1.7012500034686,0.));
#29208=CARTESIAN_POINT('Ctrl Pts',(6.56268467749999,4.87625000346864,0.));
#29209=CARTESIAN_POINT('Ctrl Pts',(6.56268467750008,4.74925000346872,2.13234551188562));
#29210=CARTESIAN_POINT('Ctrl Pts',(5.30932343282159,4.62225000346861,3.85744926888032));
#29211=CARTESIAN_POINT('Ctrl Pts',(4.05596218814312,4.49525000346869,5.58255302587488));
#29212=CARTESIAN_POINT('Ctrl Pts',(2.02798109407148,4.36825000346869,6.2414840269267));
#29213=CARTESIAN_POINT('Ctrl Pts',(0.,4.24125000346866,6.90041502797853));
#29214=CARTESIAN_POINT('Ctrl Pts',(-2.0279810940716,4.11425000346871,6.2414840269267));
#29215=CARTESIAN_POINT('Ctrl Pts',(-4.05596218814312,3.98725000346863,5.58255302587488));
#29216=CARTESIAN_POINT('Ctrl Pts',(-5.30932343282159,3.86025000346862,3.85744926888032));
#29217=CARTESIAN_POINT('Ctrl Pts',(-6.56268467749997,3.7332500034686,2.13234551188562));
#29218=CARTESIAN_POINT('Ctrl Pts',(-6.56268467749999,3.60625000346859,0.));
#29219=CARTESIAN_POINT('Ctrl Pts',(-6.56268467750008,3.47925000346862,-2.13234551188562));
#29220=CARTESIAN_POINT('Ctrl Pts',(-5.30932343282159,3.3522500034685,-3.85744926888032));
#29221=CARTESIAN_POINT('Ctrl Pts',(-4.05596218814312,3.22525000346859,-5.58255302587488));
#29222=CARTESIAN_POINT('Ctrl Pts',(-2.02798109407154,3.09825000346858,-6.2414840269267));
#29223=CARTESIAN_POINT('Ctrl Pts',(5.83678785436452E-14,2.97125000346862,
-6.90041502797853));
#29224=CARTESIAN_POINT('Ctrl Pts',(2.02798109407154,2.84425000346861,-6.2414840269267));
#29225=CARTESIAN_POINT('Ctrl Pts',(4.05596218814318,2.71725000346853,-5.58255302587488));
#29226=CARTESIAN_POINT('Ctrl Pts',(5.30932343282159,2.59025000346863,-3.85744926888032));
#29227=CARTESIAN_POINT('Ctrl Pts',(6.56268467750003,2.46325000346861,-2.13234551188562));
#29228=CARTESIAN_POINT('Ctrl Pts',(6.56268467749993,2.3362500034686,0.));
#29229=CARTESIAN_POINT('Origin',(-3.44169137633799E-14,15.9887500034686,
-8.78459658321108E-14));
#29230=CARTESIAN_POINT('',(6.56268467749999,7.41625000346852,-1.50808248733868E-13));
#29231=CARTESIAN_POINT('',(6.56268467749999,6.78125000346857,-1.55501888099865E-13));
#29232=CARTESIAN_POINT('',(6.56268467749992,15.9887500034686,-1.19377083354552E-13));
#29233=CARTESIAN_POINT('Ctrl Pts',(6.56268467749999,6.78125000346857,-5.55111512312578E-14));
#29234=CARTESIAN_POINT('Ctrl Pts',(6.56268467750003,6.65425000346861,2.13234551188562));
#29235=CARTESIAN_POINT('Ctrl Pts',(5.30932343282148,6.5272500034686,3.85744926888026));
#29236=CARTESIAN_POINT('Ctrl Pts',(4.05596218814318,6.40025000346864,5.58255302587488));
#29237=CARTESIAN_POINT('Ctrl Pts',(2.0279810940716,6.27325000346862,6.24148402692665));
#29238=CARTESIAN_POINT('Ctrl Pts',(-1.1673575708729E-13,6.14625000346872,
6.90041502797853));
#29239=CARTESIAN_POINT('Ctrl Pts',(-2.0279810940716,6.01925000346865,6.2414840269267));
#29240=CARTESIAN_POINT('Ctrl Pts',(-4.05596218814324,5.89225000346851,5.58255302587488));
#29241=CARTESIAN_POINT('Ctrl Pts',(-5.30932343282159,5.76525000346861,3.85744926888032));
#29242=CARTESIAN_POINT('Ctrl Pts',(-6.56268467750003,5.63825000346866,2.13234551188562));
#29243=CARTESIAN_POINT('Ctrl Pts',(-6.56268467750004,5.51125000346864,0.));
#29244=CARTESIAN_POINT('Ctrl Pts',(-6.56268467749997,5.38425000346863,-2.13234551188562));
#29245=CARTESIAN_POINT('Ctrl Pts',(-5.30932343282148,5.25725000346872,-3.85744926888032));
#29246=CARTESIAN_POINT('Ctrl Pts',(-4.05596218814318,5.13025000346865,-5.58255302587488));
#29247=CARTESIAN_POINT('Ctrl Pts',(-2.02798109407165,5.00325000346863,-6.2414840269267));
#29248=CARTESIAN_POINT('Ctrl Pts',(0.,4.87625000346868,-6.90041502797853));
#29249=CARTESIAN_POINT('Ctrl Pts',(2.02798109407154,4.7492500034686,-6.2414840269267));
#29250=CARTESIAN_POINT('Ctrl Pts',(4.05596218814312,4.62225000346859,-5.58255302587488));
#29251=CARTESIAN_POINT('Ctrl Pts',(5.30932343282148,4.49525000346862,-3.85744926888032));
#29252=CARTESIAN_POINT('Ctrl Pts',(6.56268467750008,4.36825000346862,-2.13234551188562));
#29253=CARTESIAN_POINT('Ctrl Pts',(6.5626846775001,4.24125000346864,0.));
#29254=CARTESIAN_POINT('Ctrl Pts',(6.56268467749999,7.41625000346852,-5.55111512312578E-14));
#29255=CARTESIAN_POINT('Ctrl Pts',(6.56268467749997,7.28925000346863,2.13234551188562));
#29256=CARTESIAN_POINT('Ctrl Pts',(5.30932343282159,7.1622500034686,3.85744926888026));
#29257=CARTESIAN_POINT('Ctrl Pts',(4.05596218814312,7.0352500034686,5.58255302587488));
#29258=CARTESIAN_POINT('Ctrl Pts',(2.02798109407154,6.90825000346851,6.24148402692665));
#29259=CARTESIAN_POINT('Ctrl Pts',(0.,6.78125000346874,6.90041502797853));
#29260=CARTESIAN_POINT('Ctrl Pts',(-2.0279810940716,6.65425000346853,6.24148402692665));
#29261=CARTESIAN_POINT('Ctrl Pts',(-4.05596218814312,6.52725000346859,5.58255302587488));
#29262=CARTESIAN_POINT('Ctrl Pts',(-5.30932343282159,6.40025000346872,3.85744926888026));
#29263=CARTESIAN_POINT('Ctrl Pts',(-6.56268467749997,6.27325000346868,2.13234551188562));
#29264=CARTESIAN_POINT('Ctrl Pts',(-6.56268467749993,6.14625000346863,0.));
#29265=CARTESIAN_POINT('Ctrl Pts',(-6.56268467749991,6.01925000346865,-2.13234551188562));
#29266=CARTESIAN_POINT('Ctrl Pts',(-5.30932343282159,5.8922500034686,-3.85744926888032));
#29267=CARTESIAN_POINT('Ctrl Pts',(-4.05596218814312,5.76525000346861,-5.58255302587488));
#29268=CARTESIAN_POINT('Ctrl Pts',(-2.02798109407154,5.63825000346863,-6.2414840269267));
#29269=CARTESIAN_POINT('Ctrl Pts',(0.,5.5112500034687,-6.90041502797853));
#29270=CARTESIAN_POINT('Ctrl Pts',(2.02798109407154,5.38425000346859,-6.2414840269267));
#29271=CARTESIAN_POINT('Ctrl Pts',(4.05596218814324,5.25725000346861,-5.58255302587488));
#29272=CARTESIAN_POINT('Ctrl Pts',(5.30932343282159,5.13025000346867,-3.85744926888032));
#29273=CARTESIAN_POINT('Ctrl Pts',(6.56268467750003,5.00325000346858,-2.13234551188562));
#29274=CARTESIAN_POINT('Ctrl Pts',(6.56268467749999,4.87625000346864,0.));
#29275=CARTESIAN_POINT('Origin',(-3.44169137633799E-14,15.9887500034686,
-8.78459658321108E-14));
#29276=CARTESIAN_POINT('',(6.56268467749999,9.95625000346861,-1.32033691269879E-13));
#29277=CARTESIAN_POINT('',(6.56268467749999,9.32125000346862,-1.36727330635876E-13));
#29278=CARTESIAN_POINT('',(6.56268467749992,15.9887500034686,-1.19377083354552E-13));
#29279=CARTESIAN_POINT('Ctrl Pts',(6.56268467749999,9.32125000346862,-5.55111512312578E-14));
#29280=CARTESIAN_POINT('Ctrl Pts',(6.56268467750003,9.19425000346858,2.13234551188562));
#29281=CARTESIAN_POINT('Ctrl Pts',(5.30932343282153,9.06725000346864,3.85744926888026));
#29282=CARTESIAN_POINT('Ctrl Pts',(4.05596218814318,8.94025000346872,5.58255302587488));
#29283=CARTESIAN_POINT('Ctrl Pts',(2.02798109407165,8.81325000346872,6.24148402692665));
#29284=CARTESIAN_POINT('Ctrl Pts',(1.1673575708729E-13,8.68625000346869,
6.90041502797853));
#29285=CARTESIAN_POINT('Ctrl Pts',(-2.0279810940716,8.55925000346869,6.24148402692665));
#29286=CARTESIAN_POINT('Ctrl Pts',(-4.05596218814306,8.4322500034686,5.58255302587488));
#29287=CARTESIAN_POINT('Ctrl Pts',(-5.30932343282159,8.3052500034686,3.85744926888026));
#29288=CARTESIAN_POINT('Ctrl Pts',(-6.56268467749991,8.17825000346862,2.13234551188562));
#29289=CARTESIAN_POINT('Ctrl Pts',(-6.56268467749999,8.05125000346868,-5.55111512312578E-14));
#29290=CARTESIAN_POINT('Ctrl Pts',(-6.56268467749997,7.92425000346871,-2.13234551188562));
#29291=CARTESIAN_POINT('Ctrl Pts',(-5.30932343282159,7.79725000346859,-3.85744926888038));
#29292=CARTESIAN_POINT('Ctrl Pts',(-4.05596218814306,7.67025000346873,-5.58255302587488));
#29293=CARTESIAN_POINT('Ctrl Pts',(-2.0279810940716,7.54325000346862,-6.24148402692676));
#29294=CARTESIAN_POINT('Ctrl Pts',(-1.1673575708729E-13,7.41625000346859,
-6.90041502797853));
#29295=CARTESIAN_POINT('Ctrl Pts',(2.02798109407154,7.28925000346869,-6.24148402692676));
#29296=CARTESIAN_POINT('Ctrl Pts',(4.05596218814318,7.16225000346861,-5.58255302587488));
#29297=CARTESIAN_POINT('Ctrl Pts',(5.30932343282153,7.03525000346861,-3.85744926888038));
#29298=CARTESIAN_POINT('Ctrl Pts',(6.56268467750008,6.90825000346864,-2.13234551188562));
#29299=CARTESIAN_POINT('Ctrl Pts',(6.56268467749999,6.78125000346857,-5.55111512312578E-14));
#29300=CARTESIAN_POINT('Ctrl Pts',(6.56268467749999,9.95625000346861,-5.55111512312578E-14));
#29301=CARTESIAN_POINT('Ctrl Pts',(6.56268467750008,9.8292500034686,2.13234551188562));
#29302=CARTESIAN_POINT('Ctrl Pts',(5.30932343282164,9.70225000346864,3.85744926888026));
#29303=CARTESIAN_POINT('Ctrl Pts',(4.05596218814312,9.57525000346868,5.58255302587488));
#29304=CARTESIAN_POINT('Ctrl Pts',(2.02798109407154,9.44825000346855,6.24148402692665));
#29305=CARTESIAN_POINT('Ctrl Pts',(0.,9.32125000346853,6.90041502797853));
#29306=CARTESIAN_POINT('Ctrl Pts',(-2.02798109407154,9.19425000346857,6.24148402692665));
#29307=CARTESIAN_POINT('Ctrl Pts',(-4.05596218814312,9.06725000346862,5.58255302587488));
#29308=CARTESIAN_POINT('Ctrl Pts',(-5.30932343282159,8.9402500034686,3.85744926888026));
#29309=CARTESIAN_POINT('Ctrl Pts',(-6.56268467749997,8.81325000346859,2.13234551188562));
#29310=CARTESIAN_POINT('Ctrl Pts',(-6.56268467749999,8.68625000346862,-5.55111512312578E-14));
#29311=CARTESIAN_POINT('Ctrl Pts',(-6.56268467750003,8.55925000346873,-2.13234551188562));
#29312=CARTESIAN_POINT('Ctrl Pts',(-5.30932343282159,8.43225000346859,-3.85744926888038));
#29313=CARTESIAN_POINT('Ctrl Pts',(-4.05596218814312,8.30525000346876,-5.58255302587488));
#29314=CARTESIAN_POINT('Ctrl Pts',(-2.02798109407148,8.17825000346861,-6.24148402692676));
#29315=CARTESIAN_POINT('Ctrl Pts',(0.,8.05125000346861,-6.90041502797853));
#29316=CARTESIAN_POINT('Ctrl Pts',(2.02798109407154,7.92425000346864,-6.24148402692676));
#29317=CARTESIAN_POINT('Ctrl Pts',(4.05596218814312,7.79725000346863,-5.58255302587488));
#29318=CARTESIAN_POINT('Ctrl Pts',(5.30932343282153,7.67025000346866,-3.85744926888038));
#29319=CARTESIAN_POINT('Ctrl Pts',(6.56268467750003,7.5432500034686,-2.13234551188562));
#29320=CARTESIAN_POINT('Ctrl Pts',(6.56268467749999,7.41625000346852,-5.55111512312578E-14));
#29321=CARTESIAN_POINT('Origin',(-3.44169137633799E-14,15.9887500034686,
-8.78459658321108E-14));
#29322=CARTESIAN_POINT('',(6.56268467749999,12.4962500034686,-1.1325913380589E-13));
#29323=CARTESIAN_POINT('',(6.56268467749999,11.8612500034686,-1.17952773171887E-13));
#29324=CARTESIAN_POINT('',(6.56268467749992,15.9887500034686,-1.19377083354552E-13));
#29325=CARTESIAN_POINT('',(-4.44227809454828,14.0999999999992,4.83063096365161));
#29326=CARTESIAN_POINT('Ctrl Pts',(-4.44227809454828,14.0999999999992,4.83063096365161));
#29327=CARTESIAN_POINT('Ctrl Pts',(-4.92436112622534,14.0592572834091,4.38730442774225));
#29328=CARTESIAN_POINT('Ctrl Pts',(-5.30932343282164,14.0202500034686,3.85744926888026));
#29329=CARTESIAN_POINT('Ctrl Pts',(-6.56268467750008,13.8932500034686,2.13234551188562));
#29330=CARTESIAN_POINT('Ctrl Pts',(-6.56268467749999,13.7662500034686,-5.55111512312578E-14));
#29331=CARTESIAN_POINT('Ctrl Pts',(-6.56268467749991,13.6392500034686,-2.13234551188562));
#29332=CARTESIAN_POINT('Ctrl Pts',(-5.30932343282153,13.5122500034687,-3.85744926888038));
#29333=CARTESIAN_POINT('Ctrl Pts',(-4.05596218814324,13.3852500034686,-5.58255302587488));
#29334=CARTESIAN_POINT('Ctrl Pts',(-2.0279810940716,13.2582500034686,-6.24148402692676));
#29335=CARTESIAN_POINT('Ctrl Pts',(0.,13.1312500034686,-6.90041502797853));
#29336=CARTESIAN_POINT('Ctrl Pts',(2.02798109407148,13.0042500034686,-6.24148402692676));
#29337=CARTESIAN_POINT('Ctrl Pts',(4.05596218814312,12.8772500034686,-5.58255302587488));
#29338=CARTESIAN_POINT('Ctrl Pts',(5.30932343282159,12.7502500034686,-3.85744926888038));
#29339=CARTESIAN_POINT('Ctrl Pts',(6.56268467750003,12.6232500034687,-2.13234551188562));
#29340=CARTESIAN_POINT('Ctrl Pts',(6.56268467749999,12.4962500034686,-5.55111512312578E-14));
#29341=CARTESIAN_POINT('',(4.81439089816027,14.0999999999991,4.45987336770942));
#29342=CARTESIAN_POINT('Origin',(-3.441691376338E-14,14.1,-1.15767576442529E-13));
#29343=CARTESIAN_POINT('Ctrl Pts',(4.81439089816027,14.0999999999991,4.45987336770942));
#29344=CARTESIAN_POINT('Ctrl Pts',(3.65313308585526,13.9950232909809,5.71344013542402));
#29345=CARTESIAN_POINT('Ctrl Pts',(2.0279810940716,13.8932500034686,6.24148402692665));
#29346=CARTESIAN_POINT('Ctrl Pts',(0.,13.7662500034686,6.90041502797853));
#29347=CARTESIAN_POINT('Ctrl Pts',(-2.02798109407165,13.6392500034685,6.24148402692665));
#29348=CARTESIAN_POINT('Ctrl Pts',(-4.05596218814318,13.5122500034686,5.58255302587488));
#29349=CARTESIAN_POINT('Ctrl Pts',(-5.30932343282153,13.3852500034687,3.85744926888026));
#29350=CARTESIAN_POINT('Ctrl Pts',(-6.56268467750003,13.2582500034686,2.13234551188562));
#29351=CARTESIAN_POINT('Ctrl Pts',(-6.56268467749999,13.1312500034686,-5.55111512312578E-14));
#29352=CARTESIAN_POINT('Ctrl Pts',(-6.56268467749997,13.0042500034686,-2.13234551188562));
#29353=CARTESIAN_POINT('Ctrl Pts',(-5.30932343282153,12.8772500034686,-3.85744926888038));
#29354=CARTESIAN_POINT('Ctrl Pts',(-4.05596218814312,12.7502500034686,-5.58255302587488));
#29355=CARTESIAN_POINT('Ctrl Pts',(-2.0279810940716,12.6232500034686,-6.24148402692676));
#29356=CARTESIAN_POINT('Ctrl Pts',(0.,12.4962500034686,-6.90041502797853));
#29357=CARTESIAN_POINT('Ctrl Pts',(2.0279810940716,12.3692500034686,-6.24148402692676));
#29358=CARTESIAN_POINT('Ctrl Pts',(4.05596218814318,12.2422500034686,-5.58255302587488));
#29359=CARTESIAN_POINT('Ctrl Pts',(5.30932343282159,12.1152500034687,-3.85744926888038));
#29360=CARTESIAN_POINT('Ctrl Pts',(6.56268467749997,11.9882500034686,-2.13234551188562));
#29361=CARTESIAN_POINT('Ctrl Pts',(6.56268467749999,11.8612500034686,-5.55111512312578E-14));
#29362=CARTESIAN_POINT('Origin',(0.,14.1,-5.55111512312578E-14));
#29363=CARTESIAN_POINT('',(-2.78947815484879E-8,0.272500004048667,7.93749999999994));
#29364=CARTESIAN_POINT('',(-3.45638790716338E-15,0.,7.93749999999994));
#29365=CARTESIAN_POINT('',(-3.55422631120848E-15,14.1,7.93749999999994));
#29366=CARTESIAN_POINT('',(-4.94987878329728,0.,6.20504683952217));
#29367=CARTESIAN_POINT('Origin',(0.,0.,0.));
#29368=CARTESIAN_POINT('Ctrl Pts',(-4.94987878329744,1.70436581514721E-14,
6.20504683952194));
#29369=CARTESIAN_POINT('Ctrl Pts',(-4.25667549292712,0.0458665906117807,
6.75802771916028));
#29370=CARTESIAN_POINT('Ctrl Pts',(-3.47565525918193,0.0917588069876965,
7.19098096194794));
#29371=CARTESIAN_POINT('Ctrl Pts',(-1.80587080516957,0.179620434800973,
7.77969428478989));
#29372=CARTESIAN_POINT('Ctrl Pts',(-0.929149370029642,0.224391358575233,
7.93232159581112));
#29373=CARTESIAN_POINT('Ctrl Pts',(-0.0302270880080657,0.270934936353027,
7.93745684009137));
#29374=CARTESIAN_POINT('Ctrl Pts',(-0.0151125175043377,0.271717524794004,
7.93749999994669));
#29375=CARTESIAN_POINT('Ctrl Pts',(-2.79692859872099E-8,0.272500005489119,
7.93749999999994));
#29376=CARTESIAN_POINT('Origin',(0.,14.1,-5.55111512312578E-14));
#29377=CARTESIAN_POINT('',(-7.49723371340113E-15,2.8125000069372,7.93749999999994));
#29378=CARTESIAN_POINT('',(-1.12431348720797E-14,2.49499999999995,7.93749999999994));
#29379=CARTESIAN_POINT('',(-3.55422631120848E-15,14.1,7.93749999999994));
#29380=CARTESIAN_POINT('',(0.88166725671843,0.000478964839786718,7.88808053401317));
#29381=CARTESIAN_POINT('Ctrl Pts',(-7.59808882477842E-15,2.49499999999995,
7.93749999999994));
#29382=CARTESIAN_POINT('Ctrl Pts',(-0.106534701701732,2.48948394341324,
7.93749999999994));
#29383=CARTESIAN_POINT('Ctrl Pts',(-0.21315395270652,2.48396350910906,7.93535520617803));
#29384=CARTESIAN_POINT('Ctrl Pts',(-1.34228594263562,2.42550034310937,7.88982662120746));
#29385=CARTESIAN_POINT('Ctrl Pts',(-2.34721168757627,2.37553557083703,7.65125568505704));
#29386=CARTESIAN_POINT('Ctrl Pts',(-4.22825870273555,2.27077151458366,6.79793705051727));
#29387=CARTESIAN_POINT('Ctrl Pts',(-5.08334996593937,2.21628774610785,6.18463094346842));
#29388=CARTESIAN_POINT('Ctrl Pts',(-6.5006440608075,2.11082869779532,4.67017498961196));
#29389=CARTESIAN_POINT('Ctrl Pts',(-7.05211470405572,2.06061785769598,3.78636421494984));
#29390=CARTESIAN_POINT('Ctrl Pts',(-7.78416468054134,1.95412820878321,1.86168514739494));
#29391=CARTESIAN_POINT('Ctrl Pts',(-7.95948874980504,1.90170675886746,0.839814635989911));
#29392=CARTESIAN_POINT('Ctrl Pts',(-7.91053560277102,1.79860647469392,-1.23798658579692));
#29393=CARTESIAN_POINT('Ctrl Pts',(-7.67720704198139,1.74387420518865,-2.27364806456493));
#29394=CARTESIAN_POINT('Ctrl Pts',(-6.8314704247939,1.63698339273262,-4.16953472439706));
#29395=CARTESIAN_POINT('Ctrl Pts',(-6.23671225204487,1.58759934630578,-5.01571954257537));
#29396=CARTESIAN_POINT('Ctrl Pts',(-4.75056903822628,1.48191850347762,-6.44270058120344));
#29397=CARTESIAN_POINT('Ctrl Pts',(-3.87038529466627,1.42787839297738,-7.00689205189505));
#29398=CARTESIAN_POINT('Ctrl Pts',(-1.93767034745183,1.32377210975524,-7.76748264468355));
#29399=CARTESIAN_POINT('Ctrl Pts',(-0.902962870018193,1.27175278765581,
-7.95444092917996));
#29400=CARTESIAN_POINT('Ctrl Pts',(1.16182405218545,1.16484413422693,-7.91845833154129));
#29401=CARTESIAN_POINT('Ctrl Pts',(2.17228416507604,1.11443142888325,-7.7027904396885));
#29402=CARTESIAN_POINT('Ctrl Pts',(4.07470078447887,1.01004914709921,-6.89142896184576));
#29403=CARTESIAN_POINT('Ctrl Pts',(4.94522720243699,0.95546296623569,-6.29600243658385));
#29404=CARTESIAN_POINT('Ctrl Pts',(6.39520826785213,0.84959255811601,-4.81301969746863));
#29405=CARTESIAN_POINT('Ctrl Pts',(6.96489277772095,0.79976927479356,-3.94386632210488));
#29406=CARTESIAN_POINT('Ctrl Pts',(7.74048137895843,0.693447126005146,-2.03673531687382));
#29407=CARTESIAN_POINT('Ctrl Pts',(7.93904769780024,0.640105599508897,-1.01701563326462));
#29408=CARTESIAN_POINT('Ctrl Pts',(7.9358969039521,0.537499009768316,1.06564198487979));
#29409=CARTESIAN_POINT('Ctrl Pts',(7.72452902037416,0.482767432371596,2.10842486523428));
#29410=CARTESIAN_POINT('Ctrl Pts',(6.91858062214297,0.375587045120146,4.02312003574284));
#29411=CARTESIAN_POINT('Ctrl Pts',(6.34250275689357,0.326128354483776,4.88107987113842));
#29412=CARTESIAN_POINT('Ctrl Pts',(4.98338043591633,0.227734503988947,6.24345275873069));
#29413=CARTESIAN_POINT('Ctrl Pts',(4.24352647010551,0.180775850154573,6.76810771789779));
#29414=CARTESIAN_POINT('Ctrl Pts',(2.62859963071464,0.0895653404014116,
7.54236428387094));
#29415=CARTESIAN_POINT('Ctrl Pts',(1.7666268132614,0.0464707913374984,7.78946812604573));
#29416=CARTESIAN_POINT('Ctrl Pts',(0.881700526094189,0.000651885411669714,
7.88837818770654));
#29417=CARTESIAN_POINT('Origin',(0.,0.,0.));
#29418=CARTESIAN_POINT('Ctrl Pts',(-2.79692896620887E-8,0.27250000548912,
7.93749999999994));
#29419=CARTESIAN_POINT('Ctrl Pts',(1.02412154774647,0.325526038068978,7.93750000360863));
#29420=CARTESIAN_POINT('Ctrl Pts',(2.0387743641584,0.376365153729017,7.73929238383186));
#29421=CARTESIAN_POINT('Ctrl Pts',(3.94831443777299,0.479964935848212,6.96344702576656));
#29422=CARTESIAN_POINT('Ctrl Pts',(4.82309953976759,0.53409799306983,6.38877090097829));
#29423=CARTESIAN_POINT('Ctrl Pts',(6.29329637177878,0.639639085112315,4.94443350923145));
#29424=CARTESIAN_POINT('Ctrl Pts',(6.87813000252512,0.689048938516753,4.09198074679249));
#29425=CARTESIAN_POINT('Ctrl Pts',(7.70277391587344,0.796096903334889,2.18604928342826));
#29426=CARTESIAN_POINT('Ctrl Pts',(7.9244674559821,0.850831949473949,1.14655097083738));
#29427=CARTESIAN_POINT('Ctrl Pts',(7.94912711678267,0.953674005975883,-0.933899729577854));
#29428=CARTESIAN_POINT('Ctrl Pts',(7.7614822973542,1.00656859984863,-1.95464195119927));
#29429=CARTESIAN_POINT('Ctrl Pts',(7.00634204924686,1.11297098466345,-3.87004642070044));
#29430=CARTESIAN_POINT('Ctrl Pts',(6.44520621813288,1.16296152304484,-4.74609739041746));
#29431=CARTESIAN_POINT('Ctrl Pts',(5.01056431745717,1.26864189885056,-6.24394855982245));
#29432=CARTESIAN_POINT('Ctrl Pts',(4.14726051728749,1.32318316370206,-6.84784030656768));
#29433=CARTESIAN_POINT('Ctrl Pts',(2.25484001253973,1.42774930414059,-7.67900151932538));
#29434=CARTESIAN_POINT('Ctrl Pts',(1.24697763497367,1.47793513664674,-7.90546715673995));
#29435=CARTESIAN_POINT('Ctrl Pts',(-0.818918926270186,1.58490124395344,
-7.96377300246748));
#29436=CARTESIAN_POINT('Ctrl Pts',(-1.85737939696264,1.63730526353135,-7.78731526484784));
#29437=CARTESIAN_POINT('Ctrl Pts',(-3.79840205169223,1.7411723140143,-7.0460200063592));
#29438=CARTESIAN_POINT('Ctrl Pts',(-4.68343537172677,1.79512128670165,-6.49149802903144));
#29439=CARTESIAN_POINT('Ctrl Pts',(-6.18410980182422,1.90092303841132,-5.08054464622637));
#29440=CARTESIAN_POINT('Ctrl Pts',(-6.78796368087669,1.95031103309894,-4.24012878133037));
#29441=CARTESIAN_POINT('Ctrl Pts',(-7.65293786749182,2.05705128565345,-2.35355027905519));
#29442=CARTESIAN_POINT('Ctrl Pts',(-7.89686305876648,2.11177478655014,-1.32150992259857));
#29443=CARTESIAN_POINT('Ctrl Pts',(-7.96799812014921,2.21510366089174,0.753726048810979));
#29444=CARTESIAN_POINT('Ctrl Pts',(-7.80391197499283,2.26712255178615,1.77660274747744));
#29445=CARTESIAN_POINT('Ctrl Pts',(-7.09294351488881,2.37368876670015,3.70968647754854));
#29446=CARTESIAN_POINT('Ctrl Pts',(-6.55030875033442,2.424129501784,4.60055434305804));
#29447=CARTESIAN_POINT('Ctrl Pts',(-5.14887517025208,2.52938034840208,6.12999929094172));
#29448=CARTESIAN_POINT('Ctrl Pts',(-4.30133144570552,2.58380545143214,6.75176605311574));
#29449=CARTESIAN_POINT('Ctrl Pts',(-2.4307452917941,2.68874131300215,7.62512804046215));
#29450=CARTESIAN_POINT('Ctrl Pts',(-1.42850359914185,2.73853625089095,7.87467129731538));
#29451=CARTESIAN_POINT('Ctrl Pts',(-0.270984323521069,2.79846922786978,
7.93403405453182));
#29452=CARTESIAN_POINT('Ctrl Pts',(-0.135428510124796,2.80548791309951,
7.93749999999994));
#29453=CARTESIAN_POINT('Ctrl Pts',(-8.32667268468867E-16,2.8125000069372,
7.93749999999994));
#29454=CARTESIAN_POINT('Origin',(0.,14.1,-5.55111512312578E-14));
#29455=CARTESIAN_POINT('',(1.10208006147732E-14,5.35250000693726,7.93749999999994));
#29456=CARTESIAN_POINT('',(-7.22738880307149E-15,5.03499999999995,7.93749999999994));
#29457=CARTESIAN_POINT('',(-3.55422631120848E-15,14.1,7.93749999999994));
#29458=CARTESIAN_POINT('Ctrl Pts',(-1.17961196366423E-15,5.03499999999995,
7.93749999999994));
#29459=CARTESIAN_POINT('Ctrl Pts',(-0.226056844747033,5.02329543493787,
7.93749999999994));
#29460=CARTESIAN_POINT('Ctrl Pts',(-0.452379981654991,5.01157708204239,
7.92784321473083));
#29461=CARTESIAN_POINT('Ctrl Pts',(-1.69853655960008,4.947054723693,7.82095339854726));
#29462=CARTESIAN_POINT('Ctrl Pts',(-2.6921904106198,4.89760386074584,7.53687454437464));
#29463=CARTESIAN_POINT('Ctrl Pts',(-4.52891436082978,4.79217528936648,6.60071567731681));
#29464=CARTESIAN_POINT('Ctrl Pts',(-5.35207911040713,4.73797561325999,5.95280125645727));
#29465=CARTESIAN_POINT('Ctrl Pts',(-6.70276294413308,4.63342744729077,4.37659409265729));
#29466=CARTESIAN_POINT('Ctrl Pts',(-7.21710810124169,4.58207327562376,3.46338007109142));
#29467=CARTESIAN_POINT('Ctrl Pts',(-7.86076483457757,4.47528268385131,1.50386890641363));
#29468=CARTESIAN_POINT('Ctrl Pts',(-7.98903928992562,4.42435921525472,0.47792817090558));
#29469=CARTESIAN_POINT('Ctrl Pts',(-7.84710502319438,4.3203471014793,-1.58817861604214));
#29470=CARTESIAN_POINT('Ctrl Pts',(-7.56954932656371,4.26569170997764,-2.60790862866832));
#29471=CARTESIAN_POINT('Ctrl Pts',(-6.64331468840853,4.15947748373841,-4.46390013422808));
#29472=CARTESIAN_POINT('Ctrl Pts',(-6.01020368526993,4.10989804615902,-5.28559000969115));
#29473=CARTESIAN_POINT('Ctrl Pts',(-4.46335320716717,4.00375460524552,-6.64421480518418));
#29474=CARTESIAN_POINT('Ctrl Pts',(-3.56337460212155,3.95013741324378,-7.16726464812353));
#29475=CARTESIAN_POINT('Ctrl Pts',(-1.59627750648389,3.84708629618733,-7.84586141832399));
#29476=CARTESIAN_POINT('Ctrl Pts',(-0.545802697038318,3.79326007407786,
-7.98800042731743));
#29477=CARTESIAN_POINT('Ctrl Pts',(1.5232931001589,3.6861283196508,-7.85689892133021));
#29478=CARTESIAN_POINT('Ctrl Pts',(2.52255243854008,3.63648678265965,-7.59526468261862));
#29479=CARTESIAN_POINT('Ctrl Pts',(4.38144464657043,3.53137005857384,-6.69986454385875));
#29480=CARTESIAN_POINT('Ctrl Pts',(5.22055929268208,3.4770168359775,-6.06885801179202));
#29481=CARTESIAN_POINT('Ctrl Pts',(6.60436711088727,3.37200380269381,-4.52296740072229));
#29482=CARTESIAN_POINT('Ctrl Pts',(7.13718103546469,3.32127619533951,-3.62429831056195));
#29483=CARTESIAN_POINT('Ctrl Pts',(7.82474966412857,3.21462848967094,-1.68195664241757));
#29484=CARTESIAN_POINT('Ctrl Pts',(7.97637434681364,3.16302331891095,-0.657989380878041));
#29485=CARTESIAN_POINT('Ctrl Pts',(7.88061997857165,3.05944882039942,1.414235300993));
#29486=CARTESIAN_POINT('Ctrl Pts',(7.62496599758344,3.00474205296789,2.44212492813196));
#29487=CARTESIAN_POINT('Ctrl Pts',(6.73866486039704,2.89817682906327,4.31821949312042));
#29488=CARTESIAN_POINT('Ctrl Pts',(6.12467717832555,2.84875338277315,5.15217888300741));
#29489=CARTESIAN_POINT('Ctrl Pts',(4.6079091059117,2.74282506352654,6.54514004824095));
#29490=CARTESIAN_POINT('Ctrl Pts',(3.71758504343212,2.68898434174957,7.08882301385243));
#29491=CARTESIAN_POINT('Ctrl Pts',(1.8675327906195,2.59070996736366,7.77156304982307));
#29492=CARTESIAN_POINT('Ctrl Pts',(0.937011186526622,2.54351571032439,7.93749999999995));
#29493=CARTESIAN_POINT('Ctrl Pts',(-9.57567358739198E-15,2.49499999999995,
7.93749999999994));
#29494=CARTESIAN_POINT('Ctrl Pts',(-4.16333634234434E-15,2.8125000069372,
7.93749999999994));
#29495=CARTESIAN_POINT('Ctrl Pts',(0.909721181897195,2.85960272030027,7.93749999999994));
#29496=CARTESIAN_POINT('Ctrl Pts',(1.81373654210814,2.90566668873107,7.78108663797075));
#29497=CARTESIAN_POINT('Ctrl Pts',(3.64424968482471,3.00226123805989,7.12664934258461));
#29498=CARTESIAN_POINT('Ctrl Pts',(4.5392362914694,3.05599840263424,6.59278652117131));
#29499=CARTESIAN_POINT('Ctrl Pts',(6.07041103374227,3.16203330133122,5.21615242755506));
#29500=CARTESIAN_POINT('Ctrl Pts',(6.69352650150149,3.21151668265289,4.38803538641356));
#29501=CARTESIAN_POINT('Ctrl Pts',(7.59893998270663,3.31791773142783,2.52148478176614));
#29502=CARTESIAN_POINT('Ctrl Pts',(7.86508648870957,3.37260318787555,1.4974371550653));
#29503=CARTESIAN_POINT('Ctrl Pts',(7.98292929617928,3.47639078088845,-0.571937970385089));
#29504=CARTESIAN_POINT('Ctrl Pts',(7.84247668327009,3.52765449298243,-1.59686075637627));
#29505=CARTESIAN_POINT('Ctrl Pts',(7.1759073479399,3.63437217351313,-3.54744652171663));
#29506=CARTESIAN_POINT('Ctrl Pts',(6.65191898932525,3.68538520334025,-4.45308697984317));
#29507=CARTESIAN_POINT('Ctrl Pts',(5.28394478157752,3.79017891575786,-6.01356419840023));
#29508=CARTESIAN_POINT('Ctrl Pts',(4.4524372569872,3.8444617038164,-6.65272668325208));
#29509=CARTESIAN_POINT('Ctrl Pts',(2.60411079213653,3.94973201136799,-7.56771579529136));
#29510=CARTESIAN_POINT('Ctrl Pts',(1.60753063476577,3.99926675237762,-7.84012292478179));
#29511=CARTESIAN_POINT('Ctrl Pts',(-0.46241352356521,4.1064424324734,-7.99354811436436));
#29512=CARTESIAN_POINT('Ctrl Pts',(-1.51649999363077,4.16075470053806,-7.8619566350794));
#29513=CARTESIAN_POINT('Ctrl Pts',(-3.49128361909894,4.2635449447295,-7.20251127690883));
#29514=CARTESIAN_POINT('Ctrl Pts',(-4.39558173765205,4.31705018290556,-6.68908533484584));
#29515=CARTESIAN_POINT('Ctrl Pts',(-5.95622232017642,4.42328254049896,-5.34651934819789));
#29516=CARTESIAN_POINT('Ctrl Pts',(-6.59818375596881,4.47297351342637,-4.53054689736886));
#29517=CARTESIAN_POINT('Ctrl Pts',(-7.54275895047591,4.57901622780737,-2.68399757361333));
#29518=CARTESIAN_POINT('Ctrl Pts',(-7.83034452991218,4.63363917585889,-1.66818531220936));
#29519=CARTESIAN_POINT('Ctrl Pts',(-7.99352465257869,4.73784241199925,0.394899491477628));
#29520=CARTESIAN_POINT('Ctrl Pts',(-7.87598550089385,4.78849377474384,1.4217173195101));
#29521=CARTESIAN_POINT('Ctrl Pts',(-7.25254590669157,4.89534568767877,3.38904270923797));
#29522=CARTESIAN_POINT('Ctrl Pts',(-6.74672145740871,4.94702620518506,4.30890979566154));
#29523=CARTESIAN_POINT('Ctrl Pts',(-5.4113035717782,5.05135240747281,5.89883540859768));
#29524=CARTESIAN_POINT('Ctrl Pts',(-4.59553406191032,5.10547343952972,6.55434440221265));
#29525=CARTESIAN_POINT('Ctrl Pts',(-2.76910942515123,5.21103367106865,7.50900517322945));
#29526=CARTESIAN_POINT('Ctrl Pts',(-1.77804029525862,5.26043825874281,7.80331188071559));
#29527=CARTESIAN_POINT('Ctrl Pts',(-0.505889512850405,5.32630652129486,
7.92542383965282));
#29528=CARTESIAN_POINT('Ctrl Pts',(-0.252793739486815,5.33941108333301,
7.93749999999994));
#29529=CARTESIAN_POINT('Ctrl Pts',(1.4363510381088E-14,5.35250000693726,
7.93749999999994));
#29530=CARTESIAN_POINT('Origin',(0.,14.1,-5.55111512312578E-14));
#29531=CARTESIAN_POINT('',(5.63434544398714E-15,7.89250000693726,7.93749999999994));
#29532=CARTESIAN_POINT('',(-2.2675240134523E-14,7.575,7.93749999999994));
#29533=CARTESIAN_POINT('',(-3.55422631120848E-15,14.1,7.93749999999994));
#29534=CARTESIAN_POINT('Ctrl Pts',(-4.73232564246473E-14,7.575,7.93749999999994));
#29535=CARTESIAN_POINT('Ctrl Pts',(-0.342311658315279,7.55727609926722,
7.93749999999994));
#29536=CARTESIAN_POINT('Ctrl Pts',(-0.68497495337198,7.53953399180717,7.91535684559342));
#29537=CARTESIAN_POINT('Ctrl Pts',(-2.04235410124708,7.46925285270692,7.73844696661338));
#29538=CARTESIAN_POINT('Ctrl Pts',(-3.0236112280855,7.41986896512291,7.41029951565781));
#29539=CARTESIAN_POINT('Ctrl Pts',(-4.82911112006103,7.31308036048196,6.38647618191546));
#29540=CARTESIAN_POINT('Ctrl Pts',(-5.63104004698734,7.25835344102439,5.69200889411091));
#29541=CARTESIAN_POINT('Ctrl Pts',(-6.90319245255078,7.1550961223596,4.05012740421005));
#29542=CARTESIAN_POINT('Ctrl Pts',(-7.36861551431731,7.10295295524148,3.12432227057014));
#29543=CARTESIAN_POINT('Ctrl Pts',(-7.92014358700705,6.99690506521083,1.14995909098138));
#29544=CARTESIAN_POINT('Ctrl Pts',(-8.00228782993313,6.94696459962651,0.120382632686124));
#29545=CARTESIAN_POINT('Ctrl Pts',(-7.76903905802668,6.84217723499278,-1.93179766506519));
#29546=CARTESIAN_POINT('Ctrl Pts',(-7.44860310515051,6.78770092206101,-2.9339584031999));
#29547=CARTESIAN_POINT('Ctrl Pts',(-6.44368460688526,6.6822691959813,-4.7484933656999));
#29548=CARTESIAN_POINT('Ctrl Pts',(-5.77228890485022,6.63202939067194,-5.54526016488532));
#29549=CARTESIAN_POINT('Ctrl Pts',(-4.16609576873437,6.52552939998956,-6.83392238043234));
#29550=CARTESIAN_POINT('Ctrl Pts',(-3.24782743689049,6.47316304583865,-7.31506224175719));
#29551=CARTESIAN_POINT('Ctrl Pts',(-1.25599959302191,6.37003200100285,-7.90767582300695));
#29552=CARTESIAN_POINT('Ctrl Pts',(-0.19894036866822,6.31530055290282,-8.00431738971416));
#29553=CARTESIAN_POINT('Ctrl Pts',(1.86512324238141,6.20842935041888,-7.78302404428111));
#29554=CARTESIAN_POINT('Ctrl Pts',(2.85332960957851,6.159046298985,-7.4774775956599));
#29555=CARTESIAN_POINT('Ctrl Pts',(4.66829436124367,6.05334902427052,-6.50254065466808));
#29556=CARTESIAN_POINT('Ctrl Pts',(5.47584795883197,5.99932067348471,-5.83876876716336));
#29557=CARTESIAN_POINT('Ctrl Pts',(6.79436786783019,5.89524572787936,-4.23384092563753));
#29558=CARTESIAN_POINT('Ctrl Pts',(7.29075169436021,5.84317694306221,-3.30664622040414));
#29559=CARTESIAN_POINT('Ctrl Pts',(7.8918229539737,5.73626051584764,-1.3307427956892));
#29560=CARTESIAN_POINT('Ctrl Pts',(7.997495578234,5.68587942536229,-0.302977384029888));
#29561=CARTESIAN_POINT('Ctrl Pts',(7.81082502569249,5.58147242770808,1.75661279939221));
#29562=CARTESIAN_POINT('Ctrl Pts',(7.51218622936447,5.52689184496292,2.76797332026668));
#29563=CARTESIAN_POINT('Ctrl Pts',(6.54735628589632,5.42104617759928,4.60393994857867));
#29564=CARTESIAN_POINT('Ctrl Pts',(5.89556966678131,5.371202341453,5.4135349757803));
#29565=CARTESIAN_POINT('Ctrl Pts',(4.31957594644649,5.26486945074441,6.73827251777554));
#29566=CARTESIAN_POINT('Ctrl Pts',(3.41055044889376,5.21158836949208,7.24090250175384));
#29567=CARTESIAN_POINT('Ctrl Pts',(1.64417149218024,5.1201304114449,7.8092239790489));
#29568=CARTESIAN_POINT('Ctrl Pts',(0.82385420015477,5.07765677112392,7.93749999999994));
#29569=CARTESIAN_POINT('Ctrl Pts',(-3.88578058618805E-15,5.03499999999995,
7.93749999999994));
#29570=CARTESIAN_POINT('Ctrl Pts',(1.12410081243297E-14,5.35250000693726,
7.93749999999994));
#29571=CARTESIAN_POINT('Ctrl Pts',(0.795747400676944,5.3937014898414,7.93749999999994));
#29572=CARTESIAN_POINT('Ctrl Pts',(1.58850203036173,5.43474801578022,7.8178277824124));
#29573=CARTESIAN_POINT('Ctrl Pts',(3.33309261958838,5.52507783561452,7.27674357940616));
#29574=CARTESIAN_POINT('Ctrl Pts',(4.24654561294269,5.57790716527978,6.7843777588313));
#29575=CARTESIAN_POINT('Ctrl Pts',(5.83699167769691,5.68432143404232,5.4768582264769));
#29576=CARTESIAN_POINT('Ctrl Pts',(6.49815399687296,5.73433953092022,4.67337969425469));
#29577=CARTESIAN_POINT('Ctrl Pts',(7.48220755546587,5.83999069856461,2.84760899648575));
#29578=CARTESIAN_POINT('Ctrl Pts',(7.79131248485743,5.89452468268523,1.84059542906963));
#29579=CARTESIAN_POINT('Ctrl Pts',(8.00030432227862,5.99911790400755,-0.215523862855896));
#29580=CARTESIAN_POINT('Ctrl Pts',(7.90590655801199,6.04927200587555,-1.24416836408562));
#29581=CARTESIAN_POINT('Ctrl Pts',(7.32610846746331,6.15624649883415,-3.22816302942619));
#29582=CARTESIAN_POINT('Ctrl Pts',(6.83871616481359,6.20871057345204,-4.16229300277298));
#29583=CARTESIAN_POINT('Ctrl Pts',(5.53627169395872,6.31254114570855,-5.78131711969542));
#29584=CARTESIAN_POINT('Ctrl Pts',(4.73656160992805,6.36647595409758,-6.45281104318585));
#29585=CARTESIAN_POINT('Ctrl Pts',(2.93255608983748,6.4722952489432,-7.44684143357893));
#29586=CARTESIAN_POINT('Ctrl Pts',(1.9470753922495,6.52168611371163,-7.76300370327744));
#29587=CARTESIAN_POINT('Ctrl Pts',(-0.114012506906427,6.62840324249997,
-8.00582976270103));
#29588=CARTESIAN_POINT('Ctrl Pts',(-1.1708829631323,6.6831249167361,-7.9205755090935));
#29589=CARTESIAN_POINT('Ctrl Pts',(-3.16718110901302,6.78648742079092,-7.35022657268397));
#29590=CARTESIAN_POINT('Ctrl Pts',(-4.08995031263565,6.83844847130781,-6.87963842497607));
#29591=CARTESIAN_POINT('Ctrl Pts',(-5.71088795218655,6.94502589301952,-5.60872603356154));
#29592=CARTESIAN_POINT('Ctrl Pts',(-6.39188199787461,6.99550338665362,-4.81828966055848));
#29593=CARTESIAN_POINT('Ctrl Pts',(-7.41688127095397,7.10078648989288,-3.01329749282044));
#29594=CARTESIAN_POINT('Ctrl Pts',(-7.74802851118764,7.15526953549469,-2.01448033935104));
#29595=CARTESIAN_POINT('Ctrl Pts',(-8.00418764143889,7.26072592251498,0.0438420911394408));
#29596=CARTESIAN_POINT('Ctrl Pts',(-7.93069937238232,7.31093956744832,1.08301320263485));
#29597=CARTESIAN_POINT('Ctrl Pts',(-7.3913569700335,7.4174302277125,3.07032729464053));
#29598=CARTESIAN_POINT('Ctrl Pts',(-6.93243106613093,7.46984628009873,4.00001582345517));
#29599=CARTESIAN_POINT('Ctrl Pts',(-5.6713126563452,7.57294957091596,5.65202322868132));
#29600=CARTESIAN_POINT('Ctrl Pts',(-4.8737152593873,7.62768176490096,6.35262566747103));
#29601=CARTESIAN_POINT('Ctrl Pts',(-3.07499434436709,7.73457066926074,7.38907513020429));
#29602=CARTESIAN_POINT('Ctrl Pts',(-2.0963984978319,7.78395459818715,7.72393351748084));
#29603=CARTESIAN_POINT('Ctrl Pts',(-0.722130494935735,7.85511019301398,
7.91288796105529));
#29604=CARTESIAN_POINT('Ctrl Pts',(-0.36089059047504,7.87381414320578,7.93749999999994));
#29605=CARTESIAN_POINT('Ctrl Pts',(2.15105711021124E-14,7.89250000693726,
7.93749999999994));
#29606=CARTESIAN_POINT('Origin',(0.,14.1,-5.55111512312578E-14));
#29607=CARTESIAN_POINT('',(1.93471957437057E-14,10.4325000069373,7.93749999999994));
#29608=CARTESIAN_POINT('',(-3.17393090743799E-14,10.115,7.93749999999994));
#29609=CARTESIAN_POINT('',(-3.55422631120848E-15,14.1,7.93749999999994));
#29610=CARTESIAN_POINT('Ctrl Pts',(-6.07847105982273E-14,10.115,7.93749999999995));
#29611=CARTESIAN_POINT('Ctrl Pts',(-0.458641069100447,10.0912529011698,
7.93749999999994));
#29612=CARTESIAN_POINT('Ctrl Pts',(-0.91749533059418,10.0674947638576,7.89774903451261));
#29613=CARTESIAN_POINT('Ctrl Pts',(-2.37949213000137,9.99179682744532,7.6413037997203));
#29614=CARTESIAN_POINT('Ctrl Pts',(-3.34393403904367,9.94221616601069,7.27114693454524));
#29615=CARTESIAN_POINT('Ctrl Pts',(-5.10235053238287,9.83506040630629,6.17045480967625));
#29616=CARTESIAN_POINT('Ctrl Pts',(-5.87355771397867,9.78097595121277,5.4414479144934));
#29617=CARTESIAN_POINT('Ctrl Pts',(-7.07550774143875,9.67806435335046,3.74210983253752));
#29618=CARTESIAN_POINT('Ctrl Pts',(-7.50109387229688,9.62450671837634,2.79277049347526));
#29619=CARTESIAN_POINT('Ctrl Pts',(-7.96502269082244,9.51831460222154,0.787015721554773));
#29620=CARTESIAN_POINT('Ctrl Pts',(-7.99990077643402,9.46867825178979,-0.250191428137116));
#29621=CARTESIAN_POINT('Ctrl Pts',(-7.66928610001285,9.36255558111798,-2.29785232778531));
#29622=CARTESIAN_POINT('Ctrl Pts',(-7.30005539978575,9.30791696570999,-3.28745464588663));
#29623=CARTESIAN_POINT('Ctrl Pts',(-6.21065675992449,9.2038011447894,-5.04781762740496));
#29624=CARTESIAN_POINT('Ctrl Pts',(-5.50824523766461,9.15302744259942,-5.80620494094393));
#29625=CARTESIAN_POINT('Ctrl Pts',(-3.84207252644146,9.04620348580589,-7.02295729521059));
#29626=CARTESIAN_POINT('Ctrl Pts',(-2.89078741216586,8.99467655318757,-7.46503428990422));
#29627=CARTESIAN_POINT('Ctrl Pts',(-0.873885938138244,8.89024726880558,
-7.95712065591083));
#29628=CARTESIAN_POINT('Ctrl Pts',(0.172096992937339,8.83608931891333,-8.0031079147963));
#29629=CARTESIAN_POINT('Ctrl Pts',(2.20968503930547,8.73058894406227,-7.69220686027878));
#29630=CARTESIAN_POINT('Ctrl Pts',(3.18266101044959,8.68116618949836,-7.34325526632608));
#29631=CARTESIAN_POINT('Ctrl Pts',(4.96692734416526,8.57407542163531,-6.28027790896194));
#29632=CARTESIAN_POINT('Ctrl Pts',(5.75524862147659,8.51934087651019,-5.56683073257915));
#29633=CARTESIAN_POINT('Ctrl Pts',(6.99294297133211,8.4165730217313,-3.89360469735698));
#29634=CARTESIAN_POINT('Ctrl Pts',(7.4381133042439,8.36353911669123,-2.95573212372524));
#29635=CARTESIAN_POINT('Ctrl Pts',(7.94623396652407,8.25716195000415,-0.960578242083116));
#29636=CARTESIAN_POINT('Ctrl Pts',(8.00370695894376,8.20722745802448,0.0778152885029483));
#29637=CARTESIAN_POINT('Ctrl Pts',(7.71675343248058,8.10148602972906,2.13192048341219));
#29638=CARTESIAN_POINT('Ctrl Pts',(7.36984710519358,8.04692986313322,3.12710210230098));
#29639=CARTESIAN_POINT('Ctrl Pts',(6.32112182604917,7.94242131969421,4.90865586491743));
#29640=CARTESIAN_POINT('Ctrl Pts',(5.63617464973127,7.89216652331995,5.68199097887513));
#29641=CARTESIAN_POINT('Ctrl Pts',(3.99521590435597,7.78521831887807,6.93752993327295));
#29642=CARTESIAN_POINT('Ctrl Pts',(3.05036582219345,7.73293905850887,7.40176912173894));
#29643=CARTESIAN_POINT('Ctrl Pts',(1.37502872996062,7.64619498305781,7.84798589621614));
#29644=CARTESIAN_POINT('Ctrl Pts',(0.68822505764354,7.61063428912565,7.93749999999995));
#29645=CARTESIAN_POINT('Ctrl Pts',(-5.06539254985228E-14,7.575,7.93749999999994));
#29646=CARTESIAN_POINT('Ctrl Pts',(2.2065682614425E-14,7.89250000693726,
7.93749999999994));
#29647=CARTESIAN_POINT('Ctrl Pts',(0.670234463880682,7.92720279551296,7.93749999999994));
#29648=CARTESIAN_POINT('Ctrl Pts',(1.33926411830421,7.96184320256437,7.8526050957819));
#29649=CARTESIAN_POINT('Ctrl Pts',(2.99899528290416,8.04777924853269,7.42256209273436));
#29650=CARTESIAN_POINT('Ctrl Pts',(3.94594229733037,8.09980337471834,6.96549066157424));
#29651=CARTESIAN_POINT('Ctrl Pts',(5.59508262861219,8.20671278851604,5.72248728462796));
#29652=CARTESIAN_POINT('Ctrl Pts',(6.28568674403704,8.25712238948963,4.95398167172491));
#29653=CARTESIAN_POINT('Ctrl Pts',(7.34761395585719,8.36150708669017,3.17923248220212));
#29654=CARTESIAN_POINT('Ctrl Pts',(7.70176239620213,8.41609272626145,2.185805446599));
#29655=CARTESIAN_POINT('Ctrl Pts',(8.0028739702793,8.52196072713378,0.133730110015611));
#29656=CARTESIAN_POINT('Ctrl Pts',(7.95274179886,8.57178599361545,-0.904289194325791));
#29657=CARTESIAN_POINT('Ctrl Pts',(7.45894724746318,8.6781091915952,-2.90300194306512));
#29658=CARTESIAN_POINT('Ctrl Pts',(7.02009311995133,8.73144480625242,-3.84461502766219));
#29659=CARTESIAN_POINT('Ctrl Pts',(5.79318113825769,8.83405446357269,-5.52748363661688));
#29660=CARTESIAN_POINT('Ctrl Pts',(5.0091654553918,8.88878612075992,-6.246762062927));
#29661=CARTESIAN_POINT('Ctrl Pts',(3.23158115468938,8.99596484558183,-7.32182655658592));
#29662=CARTESIAN_POINT('Ctrl Pts',(2.261178786054,9.04542275476233,-7.67719744432473));
#29663=CARTESIAN_POINT('Ctrl Pts',(0.225282078749181,9.15083555700256,-8.00187549109631));
#29664=CARTESIAN_POINT('Ctrl Pts',(-0.821676893795444,9.20504404347951,
-7.96276892182867));
#29665=CARTESIAN_POINT('Ctrl Pts',(-2.84136592469661,9.30961765943801,-7.48384049074501));
#29666=CARTESIAN_POINT('Ctrl Pts',(-3.79459828280301,9.36093547294504,-7.04856673754708));
#29667=CARTESIAN_POINT('Ctrl Pts',(-5.46846276992487,9.46771876164945,-5.84373748454541));
#29668=CARTESIAN_POINT('Ctrl Pts',(-6.17622004951641,9.51867553092367,-5.08994820655631));
#29669=CARTESIAN_POINT('Ctrl Pts',(-7.27801738319291,9.62266502984716,-3.33617908642261));
#29670=CARTESIAN_POINT('Ctrl Pts',(-7.65405982643817,9.67732382856,-2.34838016571328));
#29671=CARTESIAN_POINT('Ctrl Pts',(-7.99800884515637,9.783557562352,-0.302796444310101));
#29672=CARTESIAN_POINT('Ctrl Pts',(-7.9700067701409,9.83312568105443,0.734029790633371));
#29673=CARTESIAN_POINT('Ctrl Pts',(-7.51954531819447,9.93925837948954,2.7429537509967));
#29674=CARTESIAN_POINT('Ctrl Pts',(-7.09995207991095,9.99288819830642,3.69570617090967));
#29675=CARTESIAN_POINT('Ctrl Pts',(-5.90943326555059,10.0959691241069,5.4021971030452));
#29676=CARTESIAN_POINT('Ctrl Pts',(-5.14418327529678,10.1497406990643,6.13538192370205));
#29677=CARTESIAN_POINT('Ctrl Pts',(-3.39478789967035,10.2568671691636,7.24752814835039));
#29678=CARTESIAN_POINT('Ctrl Pts',(-2.43306750506007,10.3065228574942,7.62439934468818));
#29679=CARTESIAN_POINT('Ctrl Pts',(-0.954624042358646,10.3830723542333,
7.8944608539135));
#29680=CARTESIAN_POINT('Ctrl Pts',(-0.477232599070769,10.4077902928305,
7.93749999999994));
#29681=CARTESIAN_POINT('Ctrl Pts',(4.39925873507718E-14,10.4325000069373,
7.93749999999994));
#29682=CARTESIAN_POINT('Origin',(0.,14.1,-5.55111512312578E-14));
#29683=CARTESIAN_POINT('',(1.71352845339572E-14,12.9725000069373,7.93749999999994));
#29684=CARTESIAN_POINT('',(-2.6058228468434E-14,12.655,7.93749999999994));
#29685=CARTESIAN_POINT('',(-3.55422631120848E-15,14.1,7.93749999999994));
#29686=CARTESIAN_POINT('',(2.74837297199471,14.1000000000001,-7.44649932900082));
#29687=CARTESIAN_POINT('Ctrl Pts',(3.5527136788005E-14,12.9725000069373,
7.93749999999994));
#29688=CARTESIAN_POINT('Ctrl Pts',(0.441514761912383,12.9953603554592,7.93749999999994));
#29689=CARTESIAN_POINT('Ctrl Pts',(0.883293860395915,13.0182343905594,7.9006624651314));
#29690=CARTESIAN_POINT('Ctrl Pts',(2.33576268462579,13.093438996166,7.65557405604387));
#29691=CARTESIAN_POINT('Ctrl Pts',(3.30784468698389,13.1432450374237,7.28846560489659));
#29692=CARTESIAN_POINT('Ctrl Pts',(5.05761032906967,13.2495579450402,6.2035612026107));
#29693=CARTESIAN_POINT('Ctrl Pts',(5.81856026439151,13.3029516164402,5.49612540281248));
#29694=CARTESIAN_POINT('Ctrl Pts',(7.04227443491757,13.4055312000031,3.81060129369166));
#29695=CARTESIAN_POINT('Ctrl Pts',(7.48536577630057,13.4602620367625,2.84312496933517));
#29696=CARTESIAN_POINT('Ctrl Pts',(7.9610567611853,13.5674569903922,0.820826853952683));
#29697=CARTESIAN_POINT('Ctrl Pts',(8.00045927217651,13.6169227206054,-0.21180828650206));
#29698=CARTESIAN_POINT('Ctrl Pts',(7.68267872730624,13.7223187627277,-2.24888325280281));
#29699=CARTESIAN_POINT('Ctrl Pts',(7.32313231666238,13.7765364790642,-3.2330847874314));
#29700=CARTESIAN_POINT('Ctrl Pts',(6.32388253412427,13.8735480929797,-4.87847035940979));
#29701=CARTESIAN_POINT('Ctrl Pts',(5.7394996878338,13.9171161681885,-5.55419954457702));
#29702=CARTESIAN_POINT('Ctrl Pts',(4.36671516953879,14.0091367137029,-6.68835273608429));
#29703=CARTESIAN_POINT('Ctrl Pts',(3.58668621837271,14.0554678517837,-7.13709253708222));
#29704=CARTESIAN_POINT('Ctrl Pts',(2.74837297199447,14.1,-7.44649932900092));
#29705=CARTESIAN_POINT('',(-3.34416379519564,14.0999999999991,-7.19864395291942));
#29706=CARTESIAN_POINT('Origin',(0.,14.1,-5.55111512312578E-14));
#29707=CARTESIAN_POINT('Ctrl Pts',(-3.34416379519565,14.0999999999991,-7.19864395291943));
#29708=CARTESIAN_POINT('Ctrl Pts',(-2.53463385585193,14.0546446990372,-7.57471488127564));
#29709=CARTESIAN_POINT('Ctrl Pts',(-1.66747397020329,14.0113369458918,-7.81154239451509));
#29710=CARTESIAN_POINT('Ctrl Pts',(0.117776201608265,13.9189018912866,-7.98763914488592));
#29711=CARTESIAN_POINT('Ctrl Pts',(1.02330461842437,13.8720162670886,-7.92270143530879));
#29712=CARTESIAN_POINT('Ctrl Pts',(2.89294560306559,13.7752117019714,-7.46215127559449));
#29713=CARTESIAN_POINT('Ctrl Pts',(3.83066248839816,13.7243979284073,-7.02701411038719));
#29714=CARTESIAN_POINT('Ctrl Pts',(5.50073052807881,13.617582986142,-5.81591941690324));
#29715=CARTESIAN_POINT('Ctrl Pts',(6.21381880215461,13.566103830456,-5.04691532384178));
#29716=CARTESIAN_POINT('Ctrl Pts',(7.30246966856507,13.4616419945824,-3.27928268390965));
#29717=CARTESIAN_POINT('Ctrl Pts',(7.66803666025631,13.4074725272805,-2.29801717100145));
#29718=CARTESIAN_POINT('Ctrl Pts',(7.99895118058518,13.3019915132034,-0.263484125659655));
#29719=CARTESIAN_POINT('Ctrl Pts',(7.96619945483916,13.2525618377811,0.769599786611228));
#29720=CARTESIAN_POINT('Ctrl Pts',(7.50358141465413,13.1454511529384,2.79443427242162));
#29721=CARTESIAN_POINT('Ctrl Pts',(7.06711780140869,13.0907170380528,3.76413064667696));
#29722=CARTESIAN_POINT('Ctrl Pts',(5.85545454942371,12.9879843171251,5.45668017071748));
#29723=CARTESIAN_POINT('Ctrl Pts',(5.09981761461665,12.9348839510761,6.16879686335132));
#29724=CARTESIAN_POINT('Ctrl Pts',(3.35758310997936,12.828518746457,7.26578537214519));
#29725=CARTESIAN_POINT('Ctrl Pts',(2.38734373402949,12.7786097057428,7.63973996334981));
#29726=CARTESIAN_POINT('Ctrl Pts',(0.9184282191556,12.7025535383934,7.89766877418857));
#29727=CARTESIAN_POINT('Ctrl Pts',(0.459103976819018,12.6787710668436,7.93749999999995));
#29728=CARTESIAN_POINT('Ctrl Pts',(-4.413136522885E-14,12.655,7.93749999999994));
#29729=CARTESIAN_POINT('Origin',(100.349250287849,58.0000000000003,-5.55111512312578E-14));
#29730=CARTESIAN_POINT('',(93.7824240764952,63.3740766425393,-5.43873074039162E-14));
#29731=CARTESIAN_POINT('Origin',(97.7511740764953,56.5000000000003,-2.22044604925031E-13));
#29732=CARTESIAN_POINT('',(97.8805002878487,62.276000431186,-5.53448196339837E-14));
#29733=CARTESIAN_POINT('',(97.8805002878487,62.276000431186,-5.53448196339837E-14));
#29734=CARTESIAN_POINT('Origin',(100.349250287849,58.0000000000003,-5.55111512312578E-14));
#29735=CARTESIAN_POINT('Origin',(100.349250287849,58.0000000000003,-5.55111512312578E-14));
#29736=CARTESIAN_POINT('',(20.3135361207583,2.62592335746103,-5.57785450648505E-14));
#29737=CARTESIAN_POINT('',(12.3760361207582,16.3740766425391,-2.75518742664506E-14));
#29738=CARTESIAN_POINT('Origin',(16.3447861207583,9.50000000000001,-5.55111512312578E-14));
#29739=CARTESIAN_POINT('',(96.3805002878487,64.8740766425393,-5.52437573976652E-14));
#29740=CARTESIAN_POINT('Origin',(16.3447861207583,9.50000000000001,-5.55111512312578E-14));
#29741=CARTESIAN_POINT('Origin',(16.3447861207583,9.50000000000001,-5.55111512312578E-14));
#29742=CARTESIAN_POINT('',(16.215459909405,3.72399956881435,-5.60303715489411E-14));
#29743=CARTESIAN_POINT('',(20.3135361207583,2.62592335746103,-5.77226718584969E-14));
#29744=CARTESIAN_POINT('',(11.8805103239219,11.2323524991207,-3.23235249912074));
#29745=CARTESIAN_POINT('Origin',(13.746709909405,8.00000000000001,-5.55111512312578E-14));
#29746=CARTESIAN_POINT('',(12.1565117088869,13.8820812394808,-2.75430407740201));
#29747=CARTESIAN_POINT('Origin',(22.2987107739078,27.7500000031024,14.8125000036728));
#29748=CARTESIAN_POINT('',(12.0472108781263,14.1,-2.20150259211144));
#29749=CARTESIAN_POINT('Ctrl Pts',(12.0472108781263,14.1,-2.20150259211144));
#29750=CARTESIAN_POINT('Ctrl Pts',(12.0678843459318,14.0579048765951,-2.32254225822882));
#29751=CARTESIAN_POINT('Ctrl Pts',(12.0902925408505,14.0127946250959,-2.44179950334643));
#29752=CARTESIAN_POINT('Ctrl Pts',(12.1144581231571,13.9648546446133,-2.55934320764531));
#29753=CARTESIAN_POINT('Ctrl Pts',(12.1279271382907,13.9381346461283,-2.62485778585675));
#29754=CARTESIAN_POINT('Ctrl Pts',(12.1419425458387,13.9105347964401,-2.689840308819));
#29755=CARTESIAN_POINT('Ctrl Pts',(12.1565117088869,13.8820812394808,-2.75430407740201));
#29756=CARTESIAN_POINT('',(12.0472108781263,14.1,2.20150259211133));
#29757=CARTESIAN_POINT('Ctrl Pts',(12.0472108781263,14.1,2.20150259211132));
#29758=CARTESIAN_POINT('Ctrl Pts',(11.4907049197408,14.1,-6.03961325396085E-14));
#29759=CARTESIAN_POINT('Ctrl Pts',(12.0472108781263,14.1,-2.20150259211144));
#29760=CARTESIAN_POINT('',(12.1565117088869,13.8820812394808,2.7543040774019));
#29761=CARTESIAN_POINT('Ctrl Pts',(12.1565117088869,13.8820812394808,2.75430407740189));
#29762=CARTESIAN_POINT('Ctrl Pts',(12.1303722840449,13.9331315030524,2.6386456948073));
#29763=CARTESIAN_POINT('Ctrl Pts',(12.1060139372507,13.9814362147453,2.52131694964062));
#29764=CARTESIAN_POINT('Ctrl Pts',(12.0833998021185,14.0268345811549,2.40224286930925));
#29765=CARTESIAN_POINT('Ctrl Pts',(12.0707955071148,14.0521379765564,2.33587531525446));
#29766=CARTESIAN_POINT('Ctrl Pts',(12.058733515868,14.0765377118997,2.26896569206937));
#29767=CARTESIAN_POINT('Ctrl Pts',(12.0472108781263,14.1,2.20150259211132));
#29768=CARTESIAN_POINT('',(11.8805103239219,11.2323524991206,3.23235249912063));
#29769=CARTESIAN_POINT('Origin',(22.2987107722691,27.7500000007079,-14.8125000008489));
#29770=CARTESIAN_POINT('Origin',(13.746709909405,8.00000000000001,-5.55111512312578E-14));
#29771=CARTESIAN_POINT('Origin',(0.,14.1,-5.55111512312578E-14));
#29772=CARTESIAN_POINT('Ctrl Pts',(-4.21884749357559E-14,12.655,7.93749999999994));
#29773=CARTESIAN_POINT('Ctrl Pts',(-0.579914463779006,12.6249737179852,
7.93749999999994));
#29774=CARTESIAN_POINT('Ctrl Pts',(-1.15947748667141,12.5949656325551,7.87394595242885));
#29775=CARTESIAN_POINT('Ctrl Pts',(-2.72715977964003,12.5137956090803,7.52423713178313));
#29776=CARTESIAN_POINT('Ctrl Pts',(-3.67367098786041,12.4635073382784,7.11025260877252));
#29777=CARTESIAN_POINT('Ctrl Pts',(-5.37274800180185,12.3565676764149,5.93498728218027));
#29778=CARTESIAN_POINT('Ctrl Pts',(-6.1048637270787,12.3043463428722,5.17889833835055));
#29779=CARTESIAN_POINT('Ctrl Pts',(-7.23104489860743,12.200366936351,3.43325695867335));
#29780=CARTESIAN_POINT('Ctrl Pts',(-7.61663949860332,12.1463747744004,2.46209943522596));
#29781=CARTESIAN_POINT('Ctrl Pts',(-7.99150195866789,12.0406285218383,0.436459615612567));
#29782=CARTESIAN_POINT('Ctrl Pts',(-7.98103373474329,11.9912456527564,-0.598073328589007));
#29783=CARTESIAN_POINT('Ctrl Pts',(-7.56210694538478,11.8844344478724,-2.631022278771));
#29784=CARTESIAN_POINT('Ctrl Pts',(-7.14783970878105,11.8297061215808,-3.60781314121778));
#29785=CARTESIAN_POINT('Ctrl Pts',(-5.97652710178254,11.726482837202,-5.32343549253778));
#29786=CARTESIAN_POINT('Ctrl Pts',(-5.23858791367607,11.6742799952521,-6.05106074693906));
#29787=CARTESIAN_POINT('Ctrl Pts',(-3.52151821037508,11.5677490644444,-7.18813109666743));
#29788=CARTESIAN_POINT('Ctrl Pts',(-2.55747823859466,11.5174187748963,-7.58483040627315));
#29789=CARTESIAN_POINT('Ctrl Pts',(-0.522823087619294,11.4120702568272,
-7.98846239017354));
#29790=CARTESIAN_POINT('Ctrl Pts',(0.528861206991541,11.3576171069355,-7.98806497012856));
#29791=CARTESIAN_POINT('Ctrl Pts',(2.55402159520791,11.2527602000297,-7.58472519765813));
#29792=CARTESIAN_POINT('Ctrl Pts',(3.50954372789697,11.2028899408122,-7.19264619454136));
#29793=CARTESIAN_POINT('Ctrl Pts',(5.23841195128476,11.0958349775386,-6.05459635385751));
#29794=CARTESIAN_POINT('Ctrl Pts',(5.99012552771292,11.0427358686602,-5.31198777312635));
#29795=CARTESIAN_POINT('Ctrl Pts',(7.15451578954983,10.9392789840801,-3.58937238386304));
#29796=CARTESIAN_POINT('Ctrl Pts',(7.56035537425116,10.8854930493347,-2.62898080975064));
#29797=CARTESIAN_POINT('Ctrl Pts',(7.98007455387778,10.7795067290338,-0.613040650786056));
#29798=CARTESIAN_POINT('Ctrl Pts',(7.99240818396955,10.7300544630459,0.422884363461977));
#29799=CARTESIAN_POINT('Ctrl Pts',(7.61799584168553,10.6235764595768,2.46353045285619));
#29800=CARTESIAN_POINT('Ctrl Pts',(7.22640541893979,10.5688803811143,3.44703458659788));
#29801=CARTESIAN_POINT('Ctrl Pts',(6.09632292291776,10.4651907190041,5.18552436997988));
#29802=CARTESIAN_POINT('Ctrl Pts',(5.3763292293516,10.4137722115572,5.92874831387835));
#29803=CARTESIAN_POINT('Ctrl Pts',(3.68490340385191,10.3070866007226,7.10619693979162));
#29804=CARTESIAN_POINT('Ctrl Pts',(2.72725201401479,10.2562091665451,7.52586485362794));
#29805=CARTESIAN_POINT('Ctrl Pts',(1.15124096674424,10.174607904429,7.87484713432316));
#29806=CARTESIAN_POINT('Ctrl Pts',(0.575788488207968,10.144812651016,7.93749999999995));
#29807=CARTESIAN_POINT('Ctrl Pts',(-5.89805981832114E-14,10.115,7.93749999999994));
#29808=CARTESIAN_POINT('Ctrl Pts',(4.19109191795997E-14,10.4325000069373,
7.93749999999994));
#29809=CARTESIAN_POINT('Ctrl Pts',(0.557865244072069,10.4613846445709,7.93749999999994));
#29810=CARTESIAN_POINT('Ctrl Pts',(1.11551343313426,10.4902580437288,7.87868728685001));
#29811=CARTESIAN_POINT('Ctrl Pts',(2.67531963501286,10.5710202661449,7.54435003386203));
#29812=CARTESIAN_POINT('Ctrl Pts',(3.63494802025156,10.6217167186141,7.13173862549671));
#29813=CARTESIAN_POINT('Ctrl Pts',(5.33427756886483,10.728356179917,5.96668493147247));
#29814=CARTESIAN_POINT('Ctrl Pts',(6.05979254151313,10.7800024563114,5.22824691405044));
#29815=CARTESIAN_POINT('Ctrl Pts',(7.20259290222187,10.8835519868175,3.49673513528815));
#29816=CARTESIAN_POINT('Ctrl Pts',(7.60117704663546,10.9382608241988,2.51524429796514));
#29817=CARTESIAN_POINT('Ctrl Pts',(7.98930645957573,11.0448445082587,0.47690904840793));
#29818=CARTESIAN_POINT('Ctrl Pts',(7.98401058758636,11.0942627712914,-0.558596535002379));
#29819=CARTESIAN_POINT('Ctrl Pts',(7.57812242651015,11.200178396938,-2.57759503396377));
#29820=CARTESIAN_POINT('Ctrl Pts',(7.17850319392244,11.2540306452404,-3.54135438429488));
#29821=CARTESIAN_POINT('Ctrl Pts',(6.02588361859436,11.3576519189003,-5.27113262956091));
#29822=CARTESIAN_POINT('Ctrl Pts',(5.28023208431709,11.4104673366064,-6.01793109736661));
#29823=CARTESIAN_POINT('Ctrl Pts',(3.56056968016203,11.51748809768,-7.16752783866324));
#29824=CARTESIAN_POINT('Ctrl Pts',(2.60782998310456,11.5674741653522,-7.56639635070738));
#29825=CARTESIAN_POINT('Ctrl Pts',(0.584851620909866,11.6722180933054,-7.98425541389701));
#29826=CARTESIAN_POINT('Ctrl Pts',(-0.467546038531965,11.7267081791504,
-7.99198166929259));
#29827=CARTESIAN_POINT('Ctrl Pts',(-2.50478732152707,11.8321905996039,-7.60227911747851));
#29828=CARTESIAN_POINT('Ctrl Pts',(-3.47076794513677,11.8823769610477,-7.21265170917385));
#29829=CARTESIAN_POINT('Ctrl Pts',(-5.19568603346168,11.9888576904439,-6.08803326244125));
#29830=CARTESIAN_POINT('Ctrl Pts',(-5.93913557856266,12.0413268321481,-5.36522316328139));
#29831=CARTESIAN_POINT('Ctrl Pts',(-7.12304558585048,12.1444006137631,-3.65672997997241));
#29832=CARTESIAN_POINT('Ctrl Pts',(-7.54424276539696,12.1991335046262,-2.6820980975328));
#29833=CARTESIAN_POINT('Ctrl Pts',(-7.97679644286936,12.3060410559272,-0.651620238664076));
#29834=CARTESIAN_POINT('Ctrl Pts',(-7.9942243506473,12.35542632628,0.382469248486573));
#29835=CARTESIAN_POINT('Ctrl Pts',(-7.63307741991666,12.4610929734538,2.41094892881012));
#29836=CARTESIAN_POINT('Ctrl Pts',(-7.25371323229952,12.5151430945812,3.3853078408361));
#29837=CARTESIAN_POINT('Ctrl Pts',(-6.13923470871145,12.6192761720211,5.13787231059147));
#29838=CARTESIAN_POINT('Ctrl Pts',(-5.41307541922715,12.6712534316758,5.89802198140335));
#29839=CARTESIAN_POINT('Ctrl Pts',(-3.72307034122177,12.7781553778015,7.08453448555328));
#29840=CARTESIAN_POINT('Ctrl Pts',(-2.77930711107058,12.8285955790694,7.50515238039963));
#29841=CARTESIAN_POINT('Ctrl Pts',(-1.19600390162266,12.9105744081057,7.86986438990999));
#29842=CARTESIAN_POINT('Ctrl Pts',(-0.598244608684184,12.9415246434033,
7.93749999999995));
#29843=CARTESIAN_POINT('Ctrl Pts',(3.41393580072236E-14,12.9725000069373,
7.93749999999995));
#29844=CARTESIAN_POINT('Origin',(0.,14.1,-5.55111512312578E-14));
#29845=CARTESIAN_POINT('',(11.7464236222522,14.1,3.46459747903199));
#29846=CARTESIAN_POINT('Ctrl Pts',(12.1565117088871,13.8820812394807,2.75430407740162));
#29847=CARTESIAN_POINT('Ctrl Pts',(11.9496594695616,14.0046515569431,3.11258266557271));
#29848=CARTESIAN_POINT('Ctrl Pts',(11.7464236222522,14.1,3.46459747903198));
#29849=CARTESIAN_POINT('Origin',(0.,14.1,-5.55111512312578E-14));
#29850=CARTESIAN_POINT('Origin',(6.87335495470248,14.1000000000001,11.905));
#29851=CARTESIAN_POINT('',(13.7467099094049,2.29866609175239,0.));
#29852=CARTESIAN_POINT('Origin',(13.746709909405,8.,-5.26849434980831E-14));
#29853=CARTESIAN_POINT('',(8.87364124185536,14.1000000000001,8.44040252096795));
#29854=CARTESIAN_POINT('',(6.87335495470248,14.1000000000001,11.905));
#29855=CARTESIAN_POINT('',(6.87335495470248,12.6000000000002,11.905));
#29856=CARTESIAN_POINT('Ctrl Pts',(8.87364124185535,14.1,8.44040252096793));
#29857=CARTESIAN_POINT('Ctrl Pts',(7.93121327103568,13.6578583163328,10.0727356489016));
#29858=CARTESIAN_POINT('Ctrl Pts',(6.87335495470398,12.6000000000015,11.9049999999974));
#29859=CARTESIAN_POINT('',(6.87335495470248,1.5,11.9050000000001));
#29860=CARTESIAN_POINT('',(6.87335495470248,14.1000000000001,11.905));
#29861=CARTESIAN_POINT('',(8.8736412418553,2.22044604925031E-13,8.440402520968));
#29862=CARTESIAN_POINT('Ctrl Pts',(6.87335495470391,1.49999999999859,11.9049999999975));
#29863=CARTESIAN_POINT('Ctrl Pts',(7.93121327103561,0.442141683667228,10.0727356489018));
#29864=CARTESIAN_POINT('Ctrl Pts',(8.87364124185528,4.75454292391698E-14,
8.44040252096804));
#29865=CARTESIAN_POINT('',(11.7464236222521,0.,3.46459747903194));
#29866=CARTESIAN_POINT('',(6.87335495470248,1.11022302462516E-13,11.9050000000001));
#29867=CARTESIAN_POINT('',(13.746709909405,1.5,0.));
#29868=CARTESIAN_POINT('Ctrl Pts',(11.7464236222522,5.27371715124124E-14,
3.46459747903198));
#29869=CARTESIAN_POINT('Ctrl Pts',(12.6888515930718,0.442141683667233,1.83226435109827));
#29870=CARTESIAN_POINT('Ctrl Pts',(13.7467099094035,1.49999999999859,2.51795233061984E-12));
#29871=CARTESIAN_POINT('',(13.746709909405,14.1,-5.55111512312578E-14));
#29872=CARTESIAN_POINT('Origin',(13.746709909405,14.1,-5.55111512312578E-14));
#29873=CARTESIAN_POINT('',(11.7464236222523,14.1,-3.46459747903211));
#29874=CARTESIAN_POINT('Ctrl Pts',(11.7464236222523,14.1,-3.46459747903211));
#29875=CARTESIAN_POINT('Ctrl Pts',(11.8840862288804,14.0354153542157,-3.22615885004961));
#29876=CARTESIAN_POINT('Ctrl Pts',(12.0207522301902,13.9625255337105,-2.98944639211365));
#29877=CARTESIAN_POINT('Ctrl Pts',(12.1565117088869,13.8820812394808,-2.75430407740201));
#29878=CARTESIAN_POINT('Origin',(13.7467099094049,8.00000000000003,-1.4432899320127E-14));
#29879=CARTESIAN_POINT('',(11.7464236222521,0.,-3.46459747903194));
#29880=CARTESIAN_POINT('Ctrl Pts',(13.7467099094035,1.49999999999861,-2.52781374769102E-12));
#29881=CARTESIAN_POINT('Ctrl Pts',(12.6888515930719,0.442141683667257,-1.83226435109827));
#29882=CARTESIAN_POINT('Ctrl Pts',(11.7464236222522,7.62364532597791E-14,
-3.46459747903197));
#29883=CARTESIAN_POINT('',(8.8736412418553,0.,-8.440402520968));
#29884=CARTESIAN_POINT('',(13.746709909405,0.,0.));
#29885=CARTESIAN_POINT('',(6.87335495470243,1.49999999999995,-11.9050000000001));
#29886=CARTESIAN_POINT('Ctrl Pts',(8.87364124185533,4.80918128090362E-14,
-8.44040252096798));
#29887=CARTESIAN_POINT('Ctrl Pts',(7.93121327103565,0.442141683667221,-10.0727356489017));
#29888=CARTESIAN_POINT('Ctrl Pts',(6.87335495470394,1.49999999999859,-11.9049999999975));
#29889=CARTESIAN_POINT('',(6.87335495470248,12.6000000000001,-11.905));
#29890=CARTESIAN_POINT('',(6.87335495470248,14.1,-11.905));
#29891=CARTESIAN_POINT('',(8.8736412418553,14.1,-8.44040252096806));
#29892=CARTESIAN_POINT('Ctrl Pts',(6.87335495470396,12.6000000000015,-11.9049999999975));
#29893=CARTESIAN_POINT('Ctrl Pts',(7.93121327103563,13.6578583163328,-10.0727356489017));
#29894=CARTESIAN_POINT('Ctrl Pts',(8.87364124185529,14.1,-8.44040252096805));
#29895=CARTESIAN_POINT('',(13.746709909405,14.1,-5.55111512312578E-14));
#29896=CARTESIAN_POINT('Origin',(0.,14.1,-5.55111512312578E-14));
#29897=CARTESIAN_POINT('Origin',(0.,14.1,-5.55111512312578E-14));
#29898=CARTESIAN_POINT('',(2.87278238039673,14.0999999999999,-11.905));
#29899=CARTESIAN_POINT('Origin',(0.,14.1,-5.55111512312578E-14));
#29900=CARTESIAN_POINT('',(-2.87278238039679,14.1,-11.905));
#29901=CARTESIAN_POINT('',(0.,14.1,-11.905));
#29902=CARTESIAN_POINT('',(-8.87364124185536,14.1,-8.44040252096806));
#29903=CARTESIAN_POINT('Origin',(0.,14.1,-5.55111512312578E-14));
#29904=CARTESIAN_POINT('',(-11.7464236222523,14.1,-3.46459747903199));
#29905=CARTESIAN_POINT('',(-6.87335495470248,14.1,-11.905));
#29906=CARTESIAN_POINT('',(-11.7464236222523,14.1,3.46459747903199));
#29907=CARTESIAN_POINT('Origin',(0.,14.1,-5.55111512312578E-14));
#29908=CARTESIAN_POINT('',(-8.87364124185536,14.1000000000001,8.44040252096795));
#29909=CARTESIAN_POINT('',(-13.746709909405,14.1000000000001,-5.55111512312578E-14));
#29910=CARTESIAN_POINT('',(-2.87278238039679,14.1000000000001,11.905));
#29911=CARTESIAN_POINT('Origin',(0.,14.1,-5.55111512312578E-14));
#29912=CARTESIAN_POINT('',(2.87278238039668,14.1,11.905));
#29913=CARTESIAN_POINT('',(-6.87335495470248,14.1000000000001,11.905));
#29914=CARTESIAN_POINT('Origin',(0.,14.1,-5.55111512312578E-14));
#29915=CARTESIAN_POINT('Ctrl Pts',(4.81439089815928,14.1,4.45987336770828));
#29916=CARTESIAN_POINT('Ctrl Pts',(5.45085062221501,14.1,3.9043535918768));
#29917=CARTESIAN_POINT('Ctrl Pts',(5.88513855662796,14.1,3.30458855527548));
#29918=CARTESIAN_POINT('Ctrl Pts',(6.54523519250348,14.1,2.178289565022));
#29919=CARTESIAN_POINT('Ctrl Pts',(6.81015684136435,14.1,1.49685119003521));
#29920=CARTESIAN_POINT('Ctrl Pts',(7.07650468880845,14.1,0.257408185061271));
#29921=CARTESIAN_POINT('Ctrl Pts',(7.11305348659363,14.1000000000836,-0.220388032780179));
#29922=CARTESIAN_POINT('Ctrl Pts',(7.12185249698299,14.1000000000836,-1.09051005975987));
#29923=CARTESIAN_POINT('Ctrl Pts',(7.08061887026275,14.0999999999992,-1.56201229863969));
#29924=CARTESIAN_POINT('Ctrl Pts',(6.9072264798878,14.0999999999992,-2.49066379795867));
#29925=CARTESIAN_POINT('Ctrl Pts',(6.77543880742199,14.1,-2.94553773574212));
#29926=CARTESIAN_POINT('Ctrl Pts',(6.51181911719829,14.1,-3.60682978802007));
#29927=CARTESIAN_POINT('Ctrl Pts',(6.41224112310757,14.1,-3.82471112630172));
#29928=CARTESIAN_POINT('Ctrl Pts',(6.10972373678835,14.1,-4.40864758554243));
#29929=CARTESIAN_POINT('Ctrl Pts',(5.8837428763729,14.1,-4.76492359630792));
#29930=CARTESIAN_POINT('Ctrl Pts',(5.26565977805594,14.1,-5.58908540006088));
#29931=CARTESIAN_POINT('Ctrl Pts',(4.83647382882801,14.1,-6.03739008948846));
#29932=CARTESIAN_POINT('Ctrl Pts',(3.86571978096819,14.1,-6.83377631056592));
#29933=CARTESIAN_POINT('Ctrl Pts',(3.32495245618938,14.1,-7.17528491172701));
#29934=CARTESIAN_POINT('Ctrl Pts',(2.74837297199472,14.1,-7.44649932900086));
#29935=CARTESIAN_POINT('Ctrl Pts',(-3.34416379519642,14.1,-7.19864395292077));
#29936=CARTESIAN_POINT('Ctrl Pts',(-3.80496175909537,14.1,-6.93317036127327));
#29937=CARTESIAN_POINT('Ctrl Pts',(-4.23728703671821,14.1,-6.62113500445306));
#29938=CARTESIAN_POINT('Ctrl Pts',(-5.02490897558888,14.1,-5.91942515123866));
#29939=CARTESIAN_POINT('Ctrl Pts',(-5.37929764729192,14.1,-5.53294123412414));
#29940=CARTESIAN_POINT('Ctrl Pts',(-5.90207512304697,14.1,-4.83255037860479));
#29941=CARTESIAN_POINT('Ctrl Pts',(-6.09621395038283,14.1,-4.53270849908774));
#29942=CARTESIAN_POINT('Ctrl Pts',(-6.73632890639296,14.1,-3.36860941126136));
#29943=CARTESIAN_POINT('Ctrl Pts',(-7.03116378822683,14.0999999999992,-2.42871440474076));
#29944=CARTESIAN_POINT('Ctrl Pts',(-7.21129158371066,14.0999999999992,-0.716849514103212));
#29945=CARTESIAN_POINT('Ctrl Pts',(-7.20260496870702,14.0999999999998,0.25667633591363));
#29946=CARTESIAN_POINT('Ctrl Pts',(-6.67217509398093,14.0999999999998,2.0265111548136));
#29947=CARTESIAN_POINT('Ctrl Pts',(-6.35366664533318,14.1,2.68669863016612));
#29948=CARTESIAN_POINT('Ctrl Pts',(-5.58382739346403,14.1,3.7930184173696));
#29949=CARTESIAN_POINT('Ctrl Pts',(-5.10184834759149,14.1,4.34342875622177));
#29950=CARTESIAN_POINT('Ctrl Pts',(-4.44227809454922,14.1,4.83063096365287));
#29951=CARTESIAN_POINT('Origin',(0.,0.,0.));
#29952=CARTESIAN_POINT('',(2.87278238039684,1.11022302462516E-13,11.9050000000001));
#29953=CARTESIAN_POINT('Origin',(0.,0.,0.));
#29954=CARTESIAN_POINT('',(-2.87278238039695,1.11022302462516E-13,11.9050000000001));
#29955=CARTESIAN_POINT('',(-6.87335495470248,1.11022302462516E-13,11.9050000000001));
#29956=CARTESIAN_POINT('',(-8.87364124185519,1.66533453693773E-13,8.440402520968));
#29957=CARTESIAN_POINT('Origin',(0.,0.,0.));
#29958=CARTESIAN_POINT('',(-11.7464236222522,0.,3.46459747903194));
#29959=CARTESIAN_POINT('',(-13.746709909405,0.,0.));
#29960=CARTESIAN_POINT('',(-11.7464236222522,0.,-3.46459747903194));
#29961=CARTESIAN_POINT('Origin',(0.,0.,0.));
#29962=CARTESIAN_POINT('',(-8.87364124185519,0.,-8.44040252096812));
#29963=CARTESIAN_POINT('',(-6.87335495470248,-1.11022302462516E-13,-11.9050000000001));
#29964=CARTESIAN_POINT('',(-2.87278238039701,0.,-11.9050000000001));
#29965=CARTESIAN_POINT('Origin',(0.,0.,0.));
#29966=CARTESIAN_POINT('',(2.87278238039684,0.,-11.9050000000001));
#29967=CARTESIAN_POINT('',(6.87335495470248,0.,-11.9050000000001));
#29968=CARTESIAN_POINT('Origin',(0.,0.,0.));
#29969=CARTESIAN_POINT('Origin',(0.,0.,0.));
#29970=CARTESIAN_POINT('Ctrl Pts',(5.75296004380522,2.01337031627161E-17,
-3.15789184594319));
#29971=CARTESIAN_POINT('Ctrl Pts',(6.16805145920931,1.85363260495959E-17,
-2.56166546672911));
#29972=CARTESIAN_POINT('Ctrl Pts',(6.48269012589373,1.53992749440315E-15,
-1.90162976751356));
#29973=CARTESIAN_POINT('Ctrl Pts',(6.93094848290557,1.53992749440315E-15,
-0.352314338723844));
#29974=CARTESIAN_POINT('Ctrl Pts',(6.9735621303957,-2.29033109896044E-15,
0.431250662897198));
#29975=CARTESIAN_POINT('Ctrl Pts',(6.89132306443144,-2.30578919340332E-15,
1.96534646388369));
#29976=CARTESIAN_POINT('Ctrl Pts',(6.67510037401339,1.07986803510167E-13,
2.84128554352015));
#29977=CARTESIAN_POINT('Ctrl Pts',(6.07641308406255,1.07959211142374E-13,
4.14593238259473));
#29978=CARTESIAN_POINT('Ctrl Pts',(5.82171281817818,-4.17642667584523E-16,
4.55202544384661));
#29979=CARTESIAN_POINT('Ctrl Pts',(5.01566141664707,-4.30629552179204E-16,
5.67172768687367));
#29980=CARTESIAN_POINT('Ctrl Pts',(4.29205372561275,3.00713586736219E-16,
6.34879214397254));
#29981=CARTESIAN_POINT('Ctrl Pts',(2.52623730895339,2.62449789740603E-16,
7.45004618249224));
#29982=CARTESIAN_POINT('Ctrl Pts',(1.61227135251105,-2.22244929069149E-16,
7.73897430176318));
#29983=CARTESIAN_POINT('Ctrl Pts',(0.881575105385269,-2.28428747016988E-16,
7.88725607656427));
#29984=CARTESIAN_POINT('Ctrl Pts',(-4.94987878329725,-1.12418580016597E-16,
6.20504683952215));
#29985=CARTESIAN_POINT('Ctrl Pts',(-5.27029315480931,-1.12342428493602E-16,
5.89885818333482));
#29986=CARTESIAN_POINT('Ctrl Pts',(-5.564488656497,-2.81302745768979E-16,
5.56638595682626));
#29987=CARTESIAN_POINT('Ctrl Pts',(-6.09390465339696,-2.81302745768979E-16,
4.85636985748995));
#29988=CARTESIAN_POINT('Ctrl Pts',(-6.33453362765511,5.20414605987702E-11,
4.47177250256802));
#29989=CARTESIAN_POINT('Ctrl Pts',(-6.66809651486317,5.20414672868805E-11,
3.81063946212714));
#29990=CARTESIAN_POINT('Ctrl Pts',(-6.78350940590364,-1.77077700830533E-16,
3.54465253981978));
#29991=CARTESIAN_POINT('Ctrl Pts',(-7.21722783075047,-1.77077700830533E-16,
2.36186655823779));
#29992=CARTESIAN_POINT('Ctrl Pts',(-7.37128688497629,9.00446286223025E-16,
1.39508370515086));
#29993=CARTESIAN_POINT('Ctrl Pts',(-7.32878830602581,9.11740271284661E-16,
0.197855159856712));
#29994=CARTESIAN_POINT('Ctrl Pts',(-7.31012622920285,1.01089725039356E-13,
-0.0350591557617014));
#29995=CARTESIAN_POINT('Ctrl Pts',(-7.16601113065448,1.0110022688177E-13,
-1.13639635415202));
#29996=CARTESIAN_POINT('Ctrl Pts',(-6.89059191747676,6.30023822827895E-16,
-1.97852215970624));
#29997=CARTESIAN_POINT('Ctrl Pts',(-6.28104839707265,6.4286537953397E-16,
-3.08791508612891));
#29998=CARTESIAN_POINT('Ctrl Pts',(-6.06694326657524,-1.73558303903062E-11,
-3.41136766122037));
#29999=CARTESIAN_POINT('Ctrl Pts',(-5.64873030316675,-1.73558168339861E-11,
-3.94251068996791));
#30000=CARTESIAN_POINT('Ctrl Pts',(-5.45210843203702,-8.46568959619048E-16,
-4.16357330811727));
#30001=CARTESIAN_POINT('Ctrl Pts',(-4.64607031268313,-8.23624923925226E-16,
-4.95292977127109));
#30002=CARTESIAN_POINT('Ctrl Pts',(-3.94675564135096,-2.57359874551289E-17,
-5.41802989602537));
#30003=CARTESIAN_POINT('Ctrl Pts',(-3.17934379362958,-1.79845011350651E-17,
-5.74113257277705));
#30004=CARTESIAN_POINT('Origin',(6.87335495470248,14.1,-11.905));
#30005=CARTESIAN_POINT('',(-6.87335495470248,12.6,-11.905));
#30006=CARTESIAN_POINT('',(-6.87335495470254,1.49999999999995,-11.9050000000001));
#30007=CARTESIAN_POINT('',(-6.87335495470248,14.1,-11.905));
#30008=CARTESIAN_POINT('Ctrl Pts',(-6.87335495469956,12.6000000000015,-11.905));
#30009=CARTESIAN_POINT('Ctrl Pts',(-4.75763832203614,13.6578583163329,-11.905));
#30010=CARTESIAN_POINT('Ctrl Pts',(-2.87278238039677,14.1000000000001,-11.905));
#30011=CARTESIAN_POINT('Ctrl Pts',(2.87278238039676,14.1000000000001,-11.905));
#30012=CARTESIAN_POINT('Ctrl Pts',(4.75763832203614,13.6578583163329,-11.905));
#30013=CARTESIAN_POINT('Ctrl Pts',(6.87335495469956,12.6000000000015,-11.905));
#30014=CARTESIAN_POINT('Ctrl Pts',(6.87335495469949,1.49999999999853,-11.905));
#30015=CARTESIAN_POINT('Ctrl Pts',(4.75763832203613,0.442141683667185,-11.905));
#30016=CARTESIAN_POINT('Ctrl Pts',(2.87278238039681,1.09299837331425E-14,
-11.905));
#30017=CARTESIAN_POINT('Ctrl Pts',(-2.87278238039699,2.69150849428633E-14,
-11.905));
#30018=CARTESIAN_POINT('Ctrl Pts',(-4.75763832203628,0.442141683667205,
-11.905));
#30019=CARTESIAN_POINT('Ctrl Pts',(-6.87335495469961,1.49999999999853,-11.905));
#30020=CARTESIAN_POINT('Origin',(-6.87335495470248,14.1,-11.905));
#30021=CARTESIAN_POINT('',(-13.746709909405,12.6000000000001,-5.55111512312578E-14));
#30022=CARTESIAN_POINT('',(-13.746709909405,1.5,0.));
#30023=CARTESIAN_POINT('',(-13.746709909405,14.1000000000001,-5.55111512312578E-14));
#30024=CARTESIAN_POINT('Ctrl Pts',(-13.7467099094035,12.6000000000015,-2.58585423657939E-12));
#30025=CARTESIAN_POINT('Ctrl Pts',(-12.6888515930718,13.6578583163328,-1.83226435109829));
#30026=CARTESIAN_POINT('Ctrl Pts',(-11.7464236222522,14.1,-3.46459747903196));
#30027=CARTESIAN_POINT('Ctrl Pts',(-8.87364124185531,14.1,-8.44040252096801));
#30028=CARTESIAN_POINT('Ctrl Pts',(-7.93121327103563,13.6578583163329,-10.0727356489017));
#30029=CARTESIAN_POINT('Ctrl Pts',(-6.87335495470392,12.6000000000015,-11.9049999999975));
#30030=CARTESIAN_POINT('Ctrl Pts',(-6.87335495470394,1.49999999999851,-11.9049999999975));
#30031=CARTESIAN_POINT('Ctrl Pts',(-7.93121327103559,0.442141683667188,
-10.0727356489018));
#30032=CARTESIAN_POINT('Ctrl Pts',(-8.87364124185522,2.73249593328561E-16,
-8.44040252096814));
#30033=CARTESIAN_POINT('Ctrl Pts',(-11.7464236222522,-3.702531989602E-14,
-3.46459747903195));
#30034=CARTESIAN_POINT('Ctrl Pts',(-12.6888515930719,0.442141683667145,
-1.83226435109824));
#30035=CARTESIAN_POINT('Ctrl Pts',(-13.7467099094036,1.49999999999851,-2.48312588068041E-12));
#30036=CARTESIAN_POINT('Origin',(-13.746709909405,14.1000000000001,-5.55111512312578E-14));
#30037=CARTESIAN_POINT('',(-6.87335495470248,12.6000000000001,11.905));
#30038=CARTESIAN_POINT('',(-6.87335495470254,1.50000000000011,11.9050000000001));
#30039=CARTESIAN_POINT('',(-6.87335495470248,14.1000000000001,11.905));
#30040=CARTESIAN_POINT('Ctrl Pts',(-6.87335495470397,12.6000000000014,11.9049999999975));
#30041=CARTESIAN_POINT('Ctrl Pts',(-7.93121327103568,13.6578583163328,10.0727356489017));
#30042=CARTESIAN_POINT('Ctrl Pts',(-8.87364124185536,14.1,8.44040252096793));
#30043=CARTESIAN_POINT('Ctrl Pts',(-11.7464236222522,14.1,3.46459747903198));
#30044=CARTESIAN_POINT('Ctrl Pts',(-12.6888515930718,13.6578583163328,1.83226435109828));
#30045=CARTESIAN_POINT('Ctrl Pts',(-13.7467099094035,12.6000000000015,2.54058002098945E-12));
#30046=CARTESIAN_POINT('Ctrl Pts',(-13.7467099094036,1.49999999999852,2.48196499901576E-12));
#30047=CARTESIAN_POINT('Ctrl Pts',(-12.6888515930719,0.442141683667162,
1.83226435109823));
#30048=CARTESIAN_POINT('Ctrl Pts',(-11.7464236222522,-2.11768434829634E-14,
3.46459747903193));
#30049=CARTESIAN_POINT('Ctrl Pts',(-8.87364124185527,-5.19174227324266E-15,
8.44040252096809));
#30050=CARTESIAN_POINT('Ctrl Pts',(-7.9312132710356,0.442141683667188,10.0727356489018));
#30051=CARTESIAN_POINT('Ctrl Pts',(-6.87335495470391,1.49999999999856,11.9049999999975));
#30052=CARTESIAN_POINT('Origin',(-6.87335495470248,14.1000000000001,11.905));
#30053=CARTESIAN_POINT('Ctrl Pts',(6.87335495469949,12.6000000000015,11.905));
#30054=CARTESIAN_POINT('Ctrl Pts',(4.75763832203604,13.6578583163328,11.905));
#30055=CARTESIAN_POINT('Ctrl Pts',(2.87278238039665,14.1,11.905));
#30056=CARTESIAN_POINT('Ctrl Pts',(-2.87278238039675,14.1,11.905));
#30057=CARTESIAN_POINT('Ctrl Pts',(-4.75763832203612,13.6578583163328,11.905));
#30058=CARTESIAN_POINT('Ctrl Pts',(-6.87335495469954,12.6000000000015,11.905));
#30059=CARTESIAN_POINT('Ctrl Pts',(-6.87335495469967,1.49999999999856,11.905));
#30060=CARTESIAN_POINT('Ctrl Pts',(-4.75763832203629,0.442141683667203,
11.905));
#30061=CARTESIAN_POINT('Ctrl Pts',(-2.87278238039696,1.99472203129849E-14,
11.905));
#30062=CARTESIAN_POINT('Ctrl Pts',(2.87278238039686,1.99472203129849E-14,
11.905));
#30063=CARTESIAN_POINT('Ctrl Pts',(4.75763832203619,0.442141683667202,11.905));
#30064=CARTESIAN_POINT('Ctrl Pts',(6.87335495469956,1.49999999999856,11.905));
#30065=CARTESIAN_POINT('Origin',(-5.55111512312578E-14,1.5,0.));
#30066=CARTESIAN_POINT('Origin',(-5.55111512312578E-14,1.5,0.));
#30067=CARTESIAN_POINT('Origin',(0.,14.1,-5.55111512312578E-14));
#30068=CARTESIAN_POINT('Origin',(0.,14.1,-5.55111512312578E-14));
#30069=CARTESIAN_POINT('Origin',(-5.55111512312578E-14,1.5,0.));
#30070=CARTESIAN_POINT('Origin',(0.,14.1,-5.55111512312578E-14));
#30071=CARTESIAN_POINT('Origin',(-5.55111512312578E-14,1.5,0.));
#30072=CARTESIAN_POINT('Origin',(0.,14.1,-5.55111512312578E-14));
#30073=CARTESIAN_POINT('Origin',(-5.55111512312578E-14,1.5,0.));
#30074=CARTESIAN_POINT('Origin',(0.,14.1,-5.55111512312578E-14));
#30075=CARTESIAN_POINT('Origin',(-5.55111512312578E-14,1.5,0.));
#30076=CARTESIAN_POINT('Origin',(0.,14.1,-5.55111512312578E-14));
#30077=CARTESIAN_POINT('Ctrl Pts',(-6.56268467749999,16.3062500034686,-5.55111512312578E-14));
#30078=CARTESIAN_POINT('Ctrl Pts',(-6.56268467750003,16.1792500034687,-2.13234551188562));
#30079=CARTESIAN_POINT('Ctrl Pts',(-5.30932343282159,16.0522500034687,-3.85744926888038));
#30080=CARTESIAN_POINT('Ctrl Pts',(-4.05596218814306,15.9252500034686,-5.58255302587488));
#30081=CARTESIAN_POINT('Ctrl Pts',(-2.0279810940716,15.7982500034687,-6.24148402692676));
#30082=CARTESIAN_POINT('Ctrl Pts',(-1.1673575708729E-13,15.6712500034687,
-6.90041502797853));
#30083=CARTESIAN_POINT('Ctrl Pts',(2.02798109407148,15.5442500034687,-6.24148402692676));
#30084=CARTESIAN_POINT('Ctrl Pts',(4.05596218814312,15.4172500034687,-5.58255302587488));
#30085=CARTESIAN_POINT('Ctrl Pts',(5.30932343282159,15.2902500034686,-3.85744926888038));
#30086=CARTESIAN_POINT('Ctrl Pts',(6.56268467750008,15.1632500034687,-2.13234551188562));
#30087=CARTESIAN_POINT('Ctrl Pts',(6.56268467749999,15.0362500034686,-5.55111512312578E-14));
#30088=CARTESIAN_POINT('Ctrl Pts',(6.56268467750003,14.9092500034686,2.13234551188562));
#30089=CARTESIAN_POINT('Ctrl Pts',(5.30932343282159,14.7822500034687,3.85744926888026));
#30090=CARTESIAN_POINT('Ctrl Pts',(4.05596218814318,14.6552500034686,5.58255302587488));
#30091=CARTESIAN_POINT('Ctrl Pts',(2.0279810940716,14.5282500034686,6.24148402692665));
#30092=CARTESIAN_POINT('Ctrl Pts',(0.,14.4012500034686,6.90041502797853));
#30093=CARTESIAN_POINT('Ctrl Pts',(-2.02798109407154,14.2742500034686,6.24148402692665));
#30094=CARTESIAN_POINT('Ctrl Pts',(-4.05596218814312,14.1472500034686,5.58255302587488));
#30095=CARTESIAN_POINT('Ctrl Pts',(-5.30932343282164,14.0202500034686,3.85744926888026));
#30096=CARTESIAN_POINT('Ctrl Pts',(-6.56268467750008,13.8932500034686,2.13234551188562));
#30097=CARTESIAN_POINT('Ctrl Pts',(-6.56268467749999,13.7662500034686,-5.55111512312578E-14));
#30098=CARTESIAN_POINT('Ctrl Pts',(-6.56268467749991,13.6392500034686,-2.13234551188562));
#30099=CARTESIAN_POINT('Ctrl Pts',(-5.30932343282153,13.5122500034687,-3.85744926888038));
#30100=CARTESIAN_POINT('Ctrl Pts',(-4.05596218814324,13.3852500034686,-5.58255302587488));
#30101=CARTESIAN_POINT('Ctrl Pts',(-2.0279810940716,13.2582500034686,-6.24148402692676));
#30102=CARTESIAN_POINT('Ctrl Pts',(0.,13.1312500034686,-6.90041502797853));
#30103=CARTESIAN_POINT('Ctrl Pts',(2.02798109407148,13.0042500034686,-6.24148402692676));
#30104=CARTESIAN_POINT('Ctrl Pts',(4.05596218814312,12.8772500034686,-5.58255302587488));
#30105=CARTESIAN_POINT('Ctrl Pts',(5.30932343282159,12.7502500034686,-3.85744926888038));
#30106=CARTESIAN_POINT('Ctrl Pts',(6.56268467750003,12.6232500034687,-2.13234551188562));
#30107=CARTESIAN_POINT('Ctrl Pts',(6.56268467749999,12.4962500034686,-5.55111512312578E-14));
#30108=CARTESIAN_POINT('Ctrl Pts',(6.56268467749997,12.3692500034686,2.13234551188562));
#30109=CARTESIAN_POINT('Ctrl Pts',(5.30932343282153,12.2422500034687,3.85744926888026));
#30110=CARTESIAN_POINT('Ctrl Pts',(4.05596218814312,12.1152500034686,5.58255302587488));
#30111=CARTESIAN_POINT('Ctrl Pts',(2.02798109407154,11.9882500034686,6.24148402692665));
#30112=CARTESIAN_POINT('Ctrl Pts',(0.,11.8612500034686,6.90041502797853));
#30113=CARTESIAN_POINT('Ctrl Pts',(-2.02798109407154,11.7342500034686,6.24148402692665));
#30114=CARTESIAN_POINT('Ctrl Pts',(-4.05596218814312,11.6072500034687,5.58255302587488));
#30115=CARTESIAN_POINT('Ctrl Pts',(-5.30932343282153,11.4802500034686,3.85744926888026));
#30116=CARTESIAN_POINT('Ctrl Pts',(-6.56268467749997,11.3532500034686,2.13234551188562));
#30117=CARTESIAN_POINT('Ctrl Pts',(-6.56268467749999,11.2262500034686,-5.55111512312578E-14));
#30118=CARTESIAN_POINT('Ctrl Pts',(-6.56268467750003,11.0992500034686,-2.13234551188562));
#30119=CARTESIAN_POINT('Ctrl Pts',(-5.30932343282159,10.9722500034686,-3.85744926888038));
#30120=CARTESIAN_POINT('Ctrl Pts',(-4.05596218814312,10.8452500034687,-5.58255302587488));
#30121=CARTESIAN_POINT('Ctrl Pts',(-2.0279810940716,10.7182500034686,-6.24148402692676));
#30122=CARTESIAN_POINT('Ctrl Pts',(0.,10.5912500034686,-6.90041502797853));
#30123=CARTESIAN_POINT('Ctrl Pts',(2.0279810940716,10.4642500034686,-6.24148402692676));
#30124=CARTESIAN_POINT('Ctrl Pts',(4.05596218814324,10.3372500034686,-5.58255302587488));
#30125=CARTESIAN_POINT('Ctrl Pts',(5.30932343282153,10.2102500034685,-3.85744926888038));
#30126=CARTESIAN_POINT('Ctrl Pts',(6.56268467749991,10.0832500034686,-2.13234551188562));
#30127=CARTESIAN_POINT('Ctrl Pts',(6.56268467749999,9.95625000346861,-5.55111512312578E-14));
#30128=CARTESIAN_POINT('Ctrl Pts',(6.56268467750008,9.8292500034686,2.13234551188562));
#30129=CARTESIAN_POINT('Ctrl Pts',(5.30932343282164,9.70225000346864,3.85744926888026));
#30130=CARTESIAN_POINT('Ctrl Pts',(4.05596218814312,9.57525000346868,5.58255302587488));
#30131=CARTESIAN_POINT('Ctrl Pts',(2.02798109407154,9.44825000346855,6.24148402692665));
#30132=CARTESIAN_POINT('Ctrl Pts',(0.,9.32125000346853,6.90041502797853));
#30133=CARTESIAN_POINT('Ctrl Pts',(-2.02798109407154,9.19425000346857,6.24148402692665));
#30134=CARTESIAN_POINT('Ctrl Pts',(-4.05596218814312,9.06725000346862,5.58255302587488));
#30135=CARTESIAN_POINT('Ctrl Pts',(-5.30932343282159,8.9402500034686,3.85744926888026));
#30136=CARTESIAN_POINT('Ctrl Pts',(-6.56268467749997,8.81325000346859,2.13234551188562));
#30137=CARTESIAN_POINT('Ctrl Pts',(-6.56268467749999,8.68625000346862,-5.55111512312578E-14));
#30138=CARTESIAN_POINT('Ctrl Pts',(-6.56268467750003,8.55925000346873,-2.13234551188562));
#30139=CARTESIAN_POINT('Ctrl Pts',(-5.30932343282159,8.43225000346859,-3.85744926888038));
#30140=CARTESIAN_POINT('Ctrl Pts',(-4.05596218814312,8.30525000346876,-5.58255302587488));
#30141=CARTESIAN_POINT('Ctrl Pts',(-2.02798109407148,8.17825000346861,-6.24148402692676));
#30142=CARTESIAN_POINT('Ctrl Pts',(0.,8.05125000346861,-6.90041502797853));
#30143=CARTESIAN_POINT('Ctrl Pts',(2.02798109407154,7.92425000346864,-6.24148402692676));
#30144=CARTESIAN_POINT('Ctrl Pts',(4.05596218814312,7.79725000346864,-5.58255302587488));
#30145=CARTESIAN_POINT('Ctrl Pts',(5.30932343282153,7.67025000346866,-3.85744926888038));
#30146=CARTESIAN_POINT('Ctrl Pts',(6.56268467750003,7.5432500034686,-2.13234551188562));
#30147=CARTESIAN_POINT('Ctrl Pts',(6.56268467749999,7.41625000346852,-5.55111512312578E-14));
#30148=CARTESIAN_POINT('Ctrl Pts',(6.56268467749997,7.28925000346863,2.13234551188562));
#30149=CARTESIAN_POINT('Ctrl Pts',(5.30932343282159,7.1622500034686,3.85744926888026));
#30150=CARTESIAN_POINT('Ctrl Pts',(4.05596218814312,7.0352500034686,5.58255302587488));
#30151=CARTESIAN_POINT('Ctrl Pts',(2.02798109407154,6.90825000346851,6.24148402692665));
#30152=CARTESIAN_POINT('Ctrl Pts',(0.,6.78125000346874,6.90041502797853));
#30153=CARTESIAN_POINT('Ctrl Pts',(-2.0279810940716,6.65425000346853,6.24148402692665));
#30154=CARTESIAN_POINT('Ctrl Pts',(-4.05596218814312,6.52725000346859,5.58255302587488));
#30155=CARTESIAN_POINT('Ctrl Pts',(-5.30932343282159,6.40025000346872,3.85744926888026));
#30156=CARTESIAN_POINT('Ctrl Pts',(-6.56268467749997,6.27325000346868,2.13234551188562));
#30157=CARTESIAN_POINT('Ctrl Pts',(-6.56268467749993,6.14625000346863,0.));
#30158=CARTESIAN_POINT('Ctrl Pts',(-6.56268467749991,6.01925000346865,-2.13234551188562));
#30159=CARTESIAN_POINT('Ctrl Pts',(-5.30932343282159,5.8922500034686,-3.85744926888032));
#30160=CARTESIAN_POINT('Ctrl Pts',(-4.05596218814312,5.76525000346862,-5.58255302587488));
#30161=CARTESIAN_POINT('Ctrl Pts',(-2.02798109407154,5.63825000346863,-6.2414840269267));
#30162=CARTESIAN_POINT('Ctrl Pts',(0.,5.5112500034687,-6.90041502797853));
#30163=CARTESIAN_POINT('Ctrl Pts',(2.02798109407154,5.38425000346859,-6.2414840269267));
#30164=CARTESIAN_POINT('Ctrl Pts',(4.05596218814324,5.25725000346861,-5.58255302587488));
#30165=CARTESIAN_POINT('Ctrl Pts',(5.30932343282159,5.13025000346867,-3.85744926888032));
#30166=CARTESIAN_POINT('Ctrl Pts',(6.56268467750003,5.00325000346858,-2.13234551188562));
#30167=CARTESIAN_POINT('Ctrl Pts',(6.56268467749999,4.87625000346864,0.));
#30168=CARTESIAN_POINT('Ctrl Pts',(6.56268467750008,4.74925000346872,2.13234551188562));
#30169=CARTESIAN_POINT('Ctrl Pts',(5.30932343282159,4.62225000346861,3.85744926888032));
#30170=CARTESIAN_POINT('Ctrl Pts',(4.05596218814312,4.49525000346869,5.58255302587488));
#30171=CARTESIAN_POINT('Ctrl Pts',(2.02798109407148,4.36825000346869,6.2414840269267));
#30172=CARTESIAN_POINT('Ctrl Pts',(0.,4.24125000346866,6.90041502797853));
#30173=CARTESIAN_POINT('Ctrl Pts',(-2.0279810940716,4.11425000346871,6.2414840269267));
#30174=CARTESIAN_POINT('Ctrl Pts',(-4.05596218814312,3.98725000346863,5.58255302587488));
#30175=CARTESIAN_POINT('Ctrl Pts',(-5.30932343282159,3.86025000346862,3.85744926888032));
#30176=CARTESIAN_POINT('Ctrl Pts',(-6.56268467749997,3.7332500034686,2.13234551188562));
#30177=CARTESIAN_POINT('Ctrl Pts',(-6.56268467749999,3.60625000346859,0.));
#30178=CARTESIAN_POINT('Ctrl Pts',(-6.56268467750008,3.47925000346862,-2.13234551188562));
#30179=CARTESIAN_POINT('Ctrl Pts',(-5.30932343282159,3.3522500034685,-3.85744926888032));
#30180=CARTESIAN_POINT('Ctrl Pts',(-4.05596218814312,3.22525000346859,-5.58255302587488));
#30181=CARTESIAN_POINT('Ctrl Pts',(-2.02798109407154,3.09825000346858,-6.2414840269267));
#30182=CARTESIAN_POINT('Ctrl Pts',(5.83678785436452E-14,2.97125000346862,
-6.90041502797853));
#30183=CARTESIAN_POINT('Ctrl Pts',(2.02798109407154,2.84425000346861,-6.2414840269267));
#30184=CARTESIAN_POINT('Ctrl Pts',(4.05596218814318,2.71725000346853,-5.58255302587488));
#30185=CARTESIAN_POINT('Ctrl Pts',(5.30932343282159,2.59025000346863,-3.85744926888032));
#30186=CARTESIAN_POINT('Ctrl Pts',(6.56268467750003,2.46325000346861,-2.13234551188562));
#30187=CARTESIAN_POINT('Ctrl Pts',(6.56268467749993,2.3362500034686,0.));
#30188=CARTESIAN_POINT('Ctrl Pts',(6.56268467750003,2.20925000346864,2.13234551188562));
#30189=CARTESIAN_POINT('Ctrl Pts',(5.30932343282159,2.08225000346862,3.85744926888032));
#30190=CARTESIAN_POINT('Ctrl Pts',(4.05596218814324,1.95525000346861,5.58255302587488));
#30191=CARTESIAN_POINT('Ctrl Pts',(2.02798109407148,1.82825000346865,6.2414840269267));
#30192=CARTESIAN_POINT('Ctrl Pts',(1.1673575708729E-13,1.70125000346858,
6.90041502797853));
#30193=CARTESIAN_POINT('Ctrl Pts',(-2.02798109407148,1.57425000346872,6.2414840269267));
#30194=CARTESIAN_POINT('Ctrl Pts',(-4.05596218814306,1.44725000346872,5.58255302587488));
#30195=CARTESIAN_POINT('Ctrl Pts',(-5.30932343282159,1.32025000346858,3.85744926888032));
#30196=CARTESIAN_POINT('Ctrl Pts',(-6.56268467750003,1.19325000346869,2.13234551188562));
#30197=CARTESIAN_POINT('Ctrl Pts',(-6.56268467749999,1.06625000346861,0.));
#30198=CARTESIAN_POINT('Ctrl Pts',(-6.56268467749997,0.939250003468656,
-2.13234551188562));
#30199=CARTESIAN_POINT('Ctrl Pts',(-5.30932343282164,0.812250003468629,
-3.85744926888032));
#30200=CARTESIAN_POINT('Ctrl Pts',(-4.05596218814312,0.685250003468624,
-5.58255302587488));
#30201=CARTESIAN_POINT('Ctrl Pts',(-2.02798109407154,0.558250003468708,
-6.2414840269267));
#30202=CARTESIAN_POINT('Ctrl Pts',(0.,0.431250003468709,-6.90041502797853));
#30203=CARTESIAN_POINT('Ctrl Pts',(2.02798109407154,0.30425000346862,-6.2414840269267));
#30204=CARTESIAN_POINT('Ctrl Pts',(4.05596218814306,0.177250003468736,-5.58255302587488));
#30205=CARTESIAN_POINT('Ctrl Pts',(5.30932343282159,0.0502500034685882,
-3.85744926888032));
#30206=CARTESIAN_POINT('Ctrl Pts',(6.56268467750003,-0.0767499965312958,
-2.13234551188562));
#30207=CARTESIAN_POINT('Ctrl Pts',(6.56268467749993,-0.203749996531333,
0.));
#30208=CARTESIAN_POINT('Ctrl Pts',(6.56268467749991,-0.330749996531386,
2.13234551188562));
#30209=CARTESIAN_POINT('Ctrl Pts',(5.30932343282159,-0.45774999653142,3.85744926888032));
#30210=CARTESIAN_POINT('Ctrl Pts',(4.05596218814312,-0.584749996531417,
5.58255302587488));
#30211=CARTESIAN_POINT('Ctrl Pts',(2.0279810940716,-0.711749996531397,6.2414840269267));
#30212=CARTESIAN_POINT('Ctrl Pts',(1.3927615077689,-0.751529897683364,6.44787938194943));
#30213=CARTESIAN_POINT('Ctrl Pts',(0.728985515936097,-0.793098111119581,
6.5220710126346));
#30214=CARTESIAN_POINT('Ctrl Pts',(-7.9375000000001,17.0999999999999,-5.55111512312578E-14));
#30215=CARTESIAN_POINT('Ctrl Pts',(-7.93750000000009,16.973,-2.57905008884871));
#30216=CARTESIAN_POINT('Ctrl Pts',(-6.42157239285118,16.846,-4.66554544007153));
#30217=CARTESIAN_POINT('Ctrl Pts',(-4.90564478570231,16.7190000000001,-6.7520407912943));
#30218=CARTESIAN_POINT('Ctrl Pts',(-2.45282239285105,16.592,-7.54901109809286));
#30219=CARTESIAN_POINT('Ctrl Pts',(0.,16.465,-8.34598140489129));
#30220=CARTESIAN_POINT('Ctrl Pts',(2.45282239285116,16.338,-7.54901109809286));
#30221=CARTESIAN_POINT('Ctrl Pts',(4.90564478570226,16.2110000000001,-6.7520407912943));
#30222=CARTESIAN_POINT('Ctrl Pts',(6.42157239285113,16.084,-4.66554544007153));
#30223=CARTESIAN_POINT('Ctrl Pts',(7.93750000000003,15.9569999999999,-2.57905008884871));
#30224=CARTESIAN_POINT('Ctrl Pts',(7.93749999999999,15.83,-5.55111512312578E-14));
#30225=CARTESIAN_POINT('Ctrl Pts',(7.93750000000009,15.703,2.57905008884871));
#30226=CARTESIAN_POINT('Ctrl Pts',(6.42157239285113,15.576,4.66554544007142));
#30227=CARTESIAN_POINT('Ctrl Pts',(4.90564478570226,15.449,6.7520407912943));
#30228=CARTESIAN_POINT('Ctrl Pts',(2.45282239285122,15.3220000000001,7.54901109809275));
#30229=CARTESIAN_POINT('Ctrl Pts',(0.,15.195,8.34598140489129));
#30230=CARTESIAN_POINT('Ctrl Pts',(-2.45282239285116,15.068,7.54901109809275));
#30231=CARTESIAN_POINT('Ctrl Pts',(-4.90564478570231,14.9410000000001,6.7520407912943));
#30232=CARTESIAN_POINT('Ctrl Pts',(-6.42157239285118,14.8140000000001,4.66554544007142));
#30233=CARTESIAN_POINT('Ctrl Pts',(-7.93750000000003,14.687,2.57905008884871));
#30234=CARTESIAN_POINT('Ctrl Pts',(-7.9375000000001,14.56,-5.55111512312578E-14));
#30235=CARTESIAN_POINT('Ctrl Pts',(-7.93749999999997,14.4330000000001,-2.57905008884871));
#30236=CARTESIAN_POINT('Ctrl Pts',(-6.42157239285124,14.306,-4.66554544007153));
#30237=CARTESIAN_POINT('Ctrl Pts',(-4.90564478570231,14.179,-6.7520407912943));
#30238=CARTESIAN_POINT('Ctrl Pts',(-2.45282239285111,14.052,-7.54901109809286));
#30239=CARTESIAN_POINT('Ctrl Pts',(0.,13.9250000000001,-8.34598140489129));
#30240=CARTESIAN_POINT('Ctrl Pts',(2.45282239285116,13.798,-7.54901109809286));
#30241=CARTESIAN_POINT('Ctrl Pts',(4.90564478570226,13.671,-6.7520407912943));
#30242=CARTESIAN_POINT('Ctrl Pts',(6.42157239285113,13.544,-4.66554544007153));
#30243=CARTESIAN_POINT('Ctrl Pts',(7.93750000000003,13.4170000000001,-2.57905008884871));
#30244=CARTESIAN_POINT('Ctrl Pts',(7.93749999999999,13.29,-5.55111512312578E-14));
#30245=CARTESIAN_POINT('Ctrl Pts',(7.93750000000003,13.1630000000001,2.57905008884871));
#30246=CARTESIAN_POINT('Ctrl Pts',(6.42157239285113,13.036,4.66554544007142));
#30247=CARTESIAN_POINT('Ctrl Pts',(4.90564478570226,12.9090000000001,6.7520407912943));
#30248=CARTESIAN_POINT('Ctrl Pts',(2.45282239285116,12.7820000000001,7.54901109809275));
#30249=CARTESIAN_POINT('Ctrl Pts',(0.,12.6550000000001,8.34598140489129));
#30250=CARTESIAN_POINT('Ctrl Pts',(-2.45282239285116,12.528,7.54901109809275));
#30251=CARTESIAN_POINT('Ctrl Pts',(-4.9056447857022,12.401,6.7520407912943));
#30252=CARTESIAN_POINT('Ctrl Pts',(-6.42157239285124,12.274,4.66554544007142));
#30253=CARTESIAN_POINT('Ctrl Pts',(-7.93750000000003,12.1470000000001,2.57905008884871));
#30254=CARTESIAN_POINT('Ctrl Pts',(-7.9375000000001,12.0200000000001,-5.55111512312578E-14));
#30255=CARTESIAN_POINT('Ctrl Pts',(-7.93749999999997,11.8930000000001,-2.57905008884871));
#30256=CARTESIAN_POINT('Ctrl Pts',(-6.42157239285124,11.766,-4.66554544007153));
#30257=CARTESIAN_POINT('Ctrl Pts',(-4.90564478570231,11.639,-6.7520407912943));
#30258=CARTESIAN_POINT('Ctrl Pts',(-2.45282239285111,11.512,-7.54901109809286));
#30259=CARTESIAN_POINT('Ctrl Pts',(1.1673575708729E-13,11.3850000000001,
-8.34598140489129));
#30260=CARTESIAN_POINT('Ctrl Pts',(2.45282239285116,11.258,-7.54901109809286));
#30261=CARTESIAN_POINT('Ctrl Pts',(4.90564478570231,11.131,-6.7520407912943));
#30262=CARTESIAN_POINT('Ctrl Pts',(6.42157239285113,11.004,-4.66554544007153));
#30263=CARTESIAN_POINT('Ctrl Pts',(7.93750000000003,10.877,-2.57905008884871));
#30264=CARTESIAN_POINT('Ctrl Pts',(7.93749999999999,10.75,-5.55111512312578E-14));
#30265=CARTESIAN_POINT('Ctrl Pts',(7.93749999999991,10.623,2.57905008884871));
#30266=CARTESIAN_POINT('Ctrl Pts',(6.42157239285113,10.496,4.66554544007142));
#30267=CARTESIAN_POINT('Ctrl Pts',(4.90564478570237,10.369,6.7520407912943));
#30268=CARTESIAN_POINT('Ctrl Pts',(2.45282239285116,10.242,7.54901109809275));
#30269=CARTESIAN_POINT('Ctrl Pts',(1.1673575708729E-13,10.115,8.34598140489129));
#30270=CARTESIAN_POINT('Ctrl Pts',(-2.45282239285105,9.988,7.54901109809275));
#30271=CARTESIAN_POINT('Ctrl Pts',(-4.90564478570231,9.86100000000001,6.7520407912943));
#30272=CARTESIAN_POINT('Ctrl Pts',(-6.42157239285124,9.73400000000002,4.66554544007142));
#30273=CARTESIAN_POINT('Ctrl Pts',(-7.93750000000003,9.60699999999999,2.57905008884871));
#30274=CARTESIAN_POINT('Ctrl Pts',(-7.93750000000004,9.48000000000004,-5.55111512312578E-14));
#30275=CARTESIAN_POINT('Ctrl Pts',(-7.93749999999997,9.35300000000001,-2.57905008884871));
#30276=CARTESIAN_POINT('Ctrl Pts',(-6.42157239285124,9.22600000000001,-4.66554544007153));
#30277=CARTESIAN_POINT('Ctrl Pts',(-4.9056447857022,9.09899999999998,-6.7520407912943));
#30278=CARTESIAN_POINT('Ctrl Pts',(-2.45282239285116,8.97200000000004,-7.54901109809286));
#30279=CARTESIAN_POINT('Ctrl Pts',(0.,8.84500000000001,-8.34598140489129));
#30280=CARTESIAN_POINT('Ctrl Pts',(2.45282239285122,8.718,-7.54901109809286));
#30281=CARTESIAN_POINT('Ctrl Pts',(4.9056447857022,8.59100000000003,-6.7520407912943));
#30282=CARTESIAN_POINT('Ctrl Pts',(6.42157239285113,8.46399999999992,-4.66554544007153));
#30283=CARTESIAN_POINT('Ctrl Pts',(7.93750000000009,8.33700000000012,-2.57905008884871));
#30284=CARTESIAN_POINT('Ctrl Pts',(7.93749999999999,8.21,-5.55111512312578E-14));
#30285=CARTESIAN_POINT('Ctrl Pts',(7.93750000000003,8.08299999999997,2.57905008884871));
#30286=CARTESIAN_POINT('Ctrl Pts',(6.42157239285107,7.95600000000002,4.66554544007142));
#30287=CARTESIAN_POINT('Ctrl Pts',(4.90564478570237,7.829,6.7520407912943));
#30288=CARTESIAN_POINT('Ctrl Pts',(2.45282239285116,7.70199999999999,7.54901109809275));
#30289=CARTESIAN_POINT('Ctrl Pts',(0.,7.57500000000008,8.34598140489129));
#30290=CARTESIAN_POINT('Ctrl Pts',(-2.45282239285105,7.44800000000001,7.54901109809275));
#30291=CARTESIAN_POINT('Ctrl Pts',(-4.90564478570231,7.32100000000005,6.7520407912943));
#30292=CARTESIAN_POINT('Ctrl Pts',(-6.42157239285124,7.19399999999998,4.66554544007142));
#30293=CARTESIAN_POINT('Ctrl Pts',(-7.93749999999991,7.06700000000008,2.57905008884871));
#30294=CARTESIAN_POINT('Ctrl Pts',(-7.93749999999999,6.94,-5.55111512312578E-14));
#30295=CARTESIAN_POINT('Ctrl Pts',(-7.93749999999997,6.8130000000001,-2.57905008884871));
#30296=CARTESIAN_POINT('Ctrl Pts',(-6.42157239285113,6.68600000000008,-4.66554544007153));
#30297=CARTESIAN_POINT('Ctrl Pts',(-4.90564478570231,6.55900000000001,-6.7520407912943));
#30298=CARTESIAN_POINT('Ctrl Pts',(-2.45282239285116,6.4320000000001,-7.54901109809286));
#30299=CARTESIAN_POINT('Ctrl Pts',(-1.1673575708729E-13,6.3050000000001,
-8.34598140489129));
#30300=CARTESIAN_POINT('Ctrl Pts',(2.45282239285116,6.17799999999996,-7.54901109809286));
#30301=CARTESIAN_POINT('Ctrl Pts',(4.90564478570231,6.05100000000001,-6.7520407912943));
#30302=CARTESIAN_POINT('Ctrl Pts',(6.42157239285107,5.92399999999999,-4.66554544007147));
#30303=CARTESIAN_POINT('Ctrl Pts',(7.93749999999997,5.79700000000004,-2.57905008884871));
#30304=CARTESIAN_POINT('Ctrl Pts',(7.93749999999999,5.66999999999995,0.));
#30305=CARTESIAN_POINT('Ctrl Pts',(7.93750000000003,5.543,2.57905008884871));
#30306=CARTESIAN_POINT('Ctrl Pts',(6.42157239285107,5.41599999999998,4.66554544007147));
#30307=CARTESIAN_POINT('Ctrl Pts',(4.9056447857022,5.28900000000003,6.7520407912943));
#30308=CARTESIAN_POINT('Ctrl Pts',(2.45282239285116,5.16199999999994,7.54901109809281));
#30309=CARTESIAN_POINT('Ctrl Pts',(0.,5.035,8.34598140489129));
#30310=CARTESIAN_POINT('Ctrl Pts',(-2.45282239285111,4.90800000000008,7.54901109809281));
#30311=CARTESIAN_POINT('Ctrl Pts',(-4.90564478570226,4.78099999999997,6.7520407912943));
#30312=CARTESIAN_POINT('Ctrl Pts',(-6.42157239285113,4.65399999999999,4.66554544007147));
#30313=CARTESIAN_POINT('Ctrl Pts',(-7.93750000000003,4.52699999999999,2.57905008884871));
#30314=CARTESIAN_POINT('Ctrl Pts',(-7.93750000000004,4.39999999999996,0.));
#30315=CARTESIAN_POINT('Ctrl Pts',(-7.93750000000003,4.27300000000002,-2.57905008884871));
#30316=CARTESIAN_POINT('Ctrl Pts',(-6.42157239285118,4.14600000000004,-4.66554544007147));
#30317=CARTESIAN_POINT('Ctrl Pts',(-4.9056447857022,4.0190000000001,-6.7520407912943));
#30318=CARTESIAN_POINT('Ctrl Pts',(-2.45282239285116,3.89200000000006,-7.54901109809281));
#30319=CARTESIAN_POINT('Ctrl Pts',(0.,3.76500000000001,-8.34598140489129));
#30320=CARTESIAN_POINT('Ctrl Pts',(2.45282239285116,3.63800000000003,-7.54901109809281));
#30321=CARTESIAN_POINT('Ctrl Pts',(4.90564478570231,3.51100000000004,-6.7520407912943));
#30322=CARTESIAN_POINT('Ctrl Pts',(6.42157239285107,3.38400000000011,-4.66554544007147));
#30323=CARTESIAN_POINT('Ctrl Pts',(7.93749999999997,3.25700000000001,-2.57905008884871));
#30324=CARTESIAN_POINT('Ctrl Pts',(7.93749999999993,3.13000000000002,0.));
#30325=CARTESIAN_POINT('Ctrl Pts',(7.93750000000003,3.00299999999998,2.57905008884871));
#30326=CARTESIAN_POINT('Ctrl Pts',(6.42157239285113,2.87599999999993,4.66554544007147));
#30327=CARTESIAN_POINT('Ctrl Pts',(4.90564478570231,2.74900000000001,6.7520407912943));
#30328=CARTESIAN_POINT('Ctrl Pts',(2.45282239285116,2.62200000000001,7.54901109809281));
#30329=CARTESIAN_POINT('Ctrl Pts',(0.,2.49499999999997,8.34598140489129));
#30330=CARTESIAN_POINT('Ctrl Pts',(-2.45282239285111,2.36800000000004,7.54901109809281));
#30331=CARTESIAN_POINT('Ctrl Pts',(-4.90564478570237,2.241,6.7520407912943));
#30332=CARTESIAN_POINT('Ctrl Pts',(-6.42157239285113,2.114,4.66554544007147));
#30333=CARTESIAN_POINT('Ctrl Pts',(-7.93749999999991,1.98699999999997,2.57905008884871));
#30334=CARTESIAN_POINT('Ctrl Pts',(-7.93750000000004,1.85999999999992,0.));
#30335=CARTESIAN_POINT('Ctrl Pts',(-7.93750000000003,1.733,-2.57905008884871));
#30336=CARTESIAN_POINT('Ctrl Pts',(-6.42157239285118,1.606,-4.66554544007147));
#30337=CARTESIAN_POINT('Ctrl Pts',(-4.90564478570226,1.47900000000002,-6.7520407912943));
#30338=CARTESIAN_POINT('Ctrl Pts',(-2.45282239285116,1.35200000000002,-7.54901109809281));
#30339=CARTESIAN_POINT('Ctrl Pts',(-1.1673575708729E-13,1.22499999999999,
-8.34598140489129));
#30340=CARTESIAN_POINT('Ctrl Pts',(2.45282239285116,1.09799999999999,-7.54901109809281));
#30341=CARTESIAN_POINT('Ctrl Pts',(4.90564478570231,0.971000000000075,-6.7520407912943));
#30342=CARTESIAN_POINT('Ctrl Pts',(6.42157239285113,0.844000000000011,-4.66554544007147));
#30343=CARTESIAN_POINT('Ctrl Pts',(7.93750000000009,0.717000000000044,-2.57905008884871));
#30344=CARTESIAN_POINT('Ctrl Pts',(7.93749999999993,0.589999999999979,0.));
#30345=CARTESIAN_POINT('Ctrl Pts',(7.93750000000003,0.463000000000012,2.57905008884871));
#30346=CARTESIAN_POINT('Ctrl Pts',(6.42157239285113,0.336000000000003,4.66554544007147));
#30347=CARTESIAN_POINT('Ctrl Pts',(4.90564478570231,0.208999999999922,6.7520407912943));
#30348=CARTESIAN_POINT('Ctrl Pts',(2.45282239285111,0.082000000000082,7.54901109809281));
#30349=CARTESIAN_POINT('Ctrl Pts',(1.68453079969211,0.0422200988480285,
7.79864416916032));
#30350=CARTESIAN_POINT('Ctrl Pts',(0.881700526094189,0.000651885411683749,
7.88837818770657));
#30351=CARTESIAN_POINT('Ctrl Pts',(6.56268467749999,12.4962500034686,-5.55111512312578E-14));
#30352=CARTESIAN_POINT('Ctrl Pts',(6.56268467749997,12.3692500034686,2.13234551188562));
#30353=CARTESIAN_POINT('Ctrl Pts',(5.30932343282153,12.2422500034687,3.85744926888026));
#30354=CARTESIAN_POINT('Ctrl Pts',(4.05596218814312,12.1152500034686,5.58255302587488));
#30355=CARTESIAN_POINT('Ctrl Pts',(2.02798109407154,11.9882500034686,6.24148402692665));
#30356=CARTESIAN_POINT('Ctrl Pts',(0.,11.8612500034686,6.90041502797853));
#30357=CARTESIAN_POINT('Ctrl Pts',(-2.02798109407154,11.7342500034686,6.24148402692665));
#30358=CARTESIAN_POINT('Ctrl Pts',(-4.05596218814312,11.6072500034687,5.58255302587488));
#30359=CARTESIAN_POINT('Ctrl Pts',(-5.30932343282153,11.4802500034686,3.85744926888026));
#30360=CARTESIAN_POINT('Ctrl Pts',(-6.56268467749997,11.3532500034686,2.13234551188562));
#30361=CARTESIAN_POINT('Ctrl Pts',(-6.56268467749999,11.2262500034686,-5.55111512312578E-14));
#30362=CARTESIAN_POINT('Ctrl Pts',(-6.56268467750003,11.0992500034686,-2.13234551188562));
#30363=CARTESIAN_POINT('Ctrl Pts',(-5.30932343282159,10.9722500034686,-3.85744926888038));
#30364=CARTESIAN_POINT('Ctrl Pts',(-4.05596218814312,10.8452500034687,-5.58255302587488));
#30365=CARTESIAN_POINT('Ctrl Pts',(-2.0279810940716,10.7182500034686,-6.24148402692676));
#30366=CARTESIAN_POINT('Ctrl Pts',(0.,10.5912500034686,-6.90041502797853));
#30367=CARTESIAN_POINT('Ctrl Pts',(2.0279810940716,10.4642500034686,-6.24148402692676));
#30368=CARTESIAN_POINT('Ctrl Pts',(4.05596218814324,10.3372500034686,-5.58255302587488));
#30369=CARTESIAN_POINT('Ctrl Pts',(5.30932343282153,10.2102500034685,-3.85744926888038));
#30370=CARTESIAN_POINT('Ctrl Pts',(6.56268467749991,10.0832500034686,-2.13234551188562));
#30371=CARTESIAN_POINT('Ctrl Pts',(6.56268467749999,9.95625000346861,-5.55111512312578E-14));
#30372=CARTESIAN_POINT('Origin',(-3.44169137633799E-14,15.9887500034686,
-8.78459658321108E-14));
#30373=CARTESIAN_POINT('Ctrl Pts',(6.56268467749999,11.8612500034686,-5.55111512312578E-14));
#30374=CARTESIAN_POINT('Ctrl Pts',(6.56268467750003,11.7342500034686,2.13234551188562));
#30375=CARTESIAN_POINT('Ctrl Pts',(5.30932343282153,11.6072500034686,3.85744926888026));
#30376=CARTESIAN_POINT('Ctrl Pts',(4.05596218814324,11.4802500034687,5.58255302587488));
#30377=CARTESIAN_POINT('Ctrl Pts',(2.02798109407154,11.3532500034686,6.24148402692665));
#30378=CARTESIAN_POINT('Ctrl Pts',(1.1673575708729E-13,11.2262500034686,
6.90041502797853));
#30379=CARTESIAN_POINT('Ctrl Pts',(-2.02798109407154,11.0992500034686,6.24148402692665));
#30380=CARTESIAN_POINT('Ctrl Pts',(-4.05596218814306,10.9722500034686,5.58255302587488));
#30381=CARTESIAN_POINT('Ctrl Pts',(-5.30932343282153,10.8452500034686,3.85744926888026));
#30382=CARTESIAN_POINT('Ctrl Pts',(-6.56268467750003,10.7182500034686,2.13234551188562));
#30383=CARTESIAN_POINT('Ctrl Pts',(-6.56268467749999,10.5912500034687,-5.55111512312578E-14));
#30384=CARTESIAN_POINT('Ctrl Pts',(-6.56268467749997,10.4642500034686,-2.13234551188562));
#30385=CARTESIAN_POINT('Ctrl Pts',(-5.30932343282159,10.3372500034685,-3.85744926888038));
#30386=CARTESIAN_POINT('Ctrl Pts',(-4.05596218814318,10.2102500034686,-5.58255302587488));
#30387=CARTESIAN_POINT('Ctrl Pts',(-2.0279810940716,10.0832500034686,-6.24148402692676));
#30388=CARTESIAN_POINT('Ctrl Pts',(1.1673575708729E-13,9.95625000346861,
-6.90041502797853));
#30389=CARTESIAN_POINT('Ctrl Pts',(2.0279810940716,9.82925000346868,-6.24148402692676));
#30390=CARTESIAN_POINT('Ctrl Pts',(4.05596218814306,9.70225000346858,-5.58255302587488));
#30391=CARTESIAN_POINT('Ctrl Pts',(5.30932343282153,9.57525000346865,-3.85744926888038));
#30392=CARTESIAN_POINT('Ctrl Pts',(6.56268467749997,9.4482500034686,-2.13234551188562));
#30393=CARTESIAN_POINT('Ctrl Pts',(6.56268467749999,9.32125000346862,-5.55111512312578E-14));
#30394=CARTESIAN_POINT('Ctrl Pts',(-7.9375000000001,14.8775000069372,-5.55111512312578E-14));
#30395=CARTESIAN_POINT('Ctrl Pts',(-7.93750000000003,14.7505000069373,-2.57905008884871));
#30396=CARTESIAN_POINT('Ctrl Pts',(-6.42157239285124,14.6235000069372,-4.66554544007153));
#30397=CARTESIAN_POINT('Ctrl Pts',(-4.90564478570237,14.4965000069372,-6.7520407912943));
#30398=CARTESIAN_POINT('Ctrl Pts',(-2.45282239285111,14.3695000069372,-7.54901109809286));
#30399=CARTESIAN_POINT('Ctrl Pts',(0.,14.2425000069373,-8.34598140489129));
#30400=CARTESIAN_POINT('Ctrl Pts',(2.45282239285116,14.1155000069372,-7.54901109809286));
#30401=CARTESIAN_POINT('Ctrl Pts',(4.90564478570231,13.9885000069372,-6.7520407912943));
#30402=CARTESIAN_POINT('Ctrl Pts',(6.42157239285113,13.8615000069372,-4.66554544007153));
#30403=CARTESIAN_POINT('Ctrl Pts',(7.93749999999997,13.7345000069373,-2.57905008884871));
#30404=CARTESIAN_POINT('Ctrl Pts',(7.93749999999999,13.6075000069373,-5.55111512312578E-14));
#30405=CARTESIAN_POINT('Ctrl Pts',(7.93749999999997,13.4805000069373,2.57905008884871));
#30406=CARTESIAN_POINT('Ctrl Pts',(6.42157239285113,13.3535000069373,4.66554544007142));
#30407=CARTESIAN_POINT('Ctrl Pts',(4.90564478570231,13.2265000069373,6.7520407912943));
#30408=CARTESIAN_POINT('Ctrl Pts',(2.45282239285116,13.0995000069373,7.54901109809275));
#30409=CARTESIAN_POINT('Ctrl Pts',(0.,12.9725000069372,8.34598140489129));
#30410=CARTESIAN_POINT('Ctrl Pts',(-2.45282239285105,12.8455000069373,7.54901109809275));
#30411=CARTESIAN_POINT('Ctrl Pts',(-4.90564478570226,12.7185000069372,6.7520407912943));
#30412=CARTESIAN_POINT('Ctrl Pts',(-6.42157239285124,12.5915000069373,4.66554544007142));
#30413=CARTESIAN_POINT('Ctrl Pts',(-7.93749999999997,12.4645000069372,2.57905008884871));
#30414=CARTESIAN_POINT('Ctrl Pts',(-7.93750000000004,12.3375000069372,-5.55111512312578E-14));
#30415=CARTESIAN_POINT('Ctrl Pts',(-7.93750000000003,12.2105000069372,-2.57905008884871));
#30416=CARTESIAN_POINT('Ctrl Pts',(-6.42157239285113,12.0835000069371,-4.66554544007153));
#30417=CARTESIAN_POINT('Ctrl Pts',(-4.90564478570226,11.9565000069372,-6.7520407912943));
#30418=CARTESIAN_POINT('Ctrl Pts',(-2.45282239285111,11.8295000069372,-7.54901109809286));
#30419=CARTESIAN_POINT('Ctrl Pts',(0.,11.7025000069372,-8.34598140489129));
#30420=CARTESIAN_POINT('Ctrl Pts',(2.45282239285122,11.5755000069372,-7.54901109809286));
#30421=CARTESIAN_POINT('Ctrl Pts',(4.90564478570226,11.4485000069373,-6.7520407912943));
#30422=CARTESIAN_POINT('Ctrl Pts',(6.42157239285113,11.3215000069372,-4.66554544007153));
#30423=CARTESIAN_POINT('Ctrl Pts',(7.93750000000003,11.1945000069372,-2.57905008884871));
#30424=CARTESIAN_POINT('Ctrl Pts',(7.93749999999999,11.0675000069372,-5.55111512312578E-14));
#30425=CARTESIAN_POINT('Ctrl Pts',(7.93750000000009,10.9405000069372,2.57905008884871));
#30426=CARTESIAN_POINT('Ctrl Pts',(6.42157239285113,10.8135000069373,4.66554544007142));
#30427=CARTESIAN_POINT('Ctrl Pts',(4.90564478570231,10.6865000069372,6.7520407912943));
#30428=CARTESIAN_POINT('Ctrl Pts',(2.45282239285116,10.5595000069372,7.54901109809275));
#30429=CARTESIAN_POINT('Ctrl Pts',(0.,10.4325000069372,8.34598140489129));
#30430=CARTESIAN_POINT('Ctrl Pts',(-2.45282239285105,10.3055000069373,7.54901109809275));
#30431=CARTESIAN_POINT('Ctrl Pts',(-4.90564478570231,10.1785000069373,6.7520407912943));
#30432=CARTESIAN_POINT('Ctrl Pts',(-6.42157239285124,10.0515000069372,4.66554544007142));
#30433=CARTESIAN_POINT('Ctrl Pts',(-7.93749999999997,9.92450000693731,2.57905008884871));
#30434=CARTESIAN_POINT('Ctrl Pts',(-7.93749999999999,9.7975000069373,-5.55111512312578E-14));
#30435=CARTESIAN_POINT('Ctrl Pts',(-7.93749999999991,9.67050000693722,-2.57905008884871));
#30436=CARTESIAN_POINT('Ctrl Pts',(-6.42157239285113,9.54350000693721,-4.66554544007153));
#30437=CARTESIAN_POINT('Ctrl Pts',(-4.90564478570226,9.41650000693719,-6.7520407912943));
#30438=CARTESIAN_POINT('Ctrl Pts',(-2.45282239285116,9.28950000693724,-7.54901109809286));
#30439=CARTESIAN_POINT('Ctrl Pts',(0.,9.16250000693733,-8.34598140489129));
#30440=CARTESIAN_POINT('Ctrl Pts',(2.45282239285116,9.03550000693709,-7.54901109809286));
#30441=CARTESIAN_POINT('Ctrl Pts',(4.90564478570237,8.90850000693724,-6.7520407912943));
#30442=CARTESIAN_POINT('Ctrl Pts',(6.42157239285113,8.78150000693712,-4.66554544007153));
#30443=CARTESIAN_POINT('Ctrl Pts',(7.93750000000003,8.65450000693732,-2.57905008884871));
#30444=CARTESIAN_POINT('Ctrl Pts',(7.93749999999999,8.52750000693719,-5.55111512312578E-14));
#30445=CARTESIAN_POINT('Ctrl Pts',(7.93749999999997,8.40050000693729,2.57905008884871));
#30446=CARTESIAN_POINT('Ctrl Pts',(6.42157239285113,8.27350000693722,4.66554544007142));
#30447=CARTESIAN_POINT('Ctrl Pts',(4.90564478570231,8.14650000693721,6.7520407912943));
#30448=CARTESIAN_POINT('Ctrl Pts',(2.45282239285116,8.01950000693724,7.54901109809275));
#30449=CARTESIAN_POINT('Ctrl Pts',(1.1673575708729E-13,7.89250000693723,
8.34598140489129));
#30450=CARTESIAN_POINT('Ctrl Pts',(-2.45282239285111,7.76550000693721,7.54901109809275));
#30451=CARTESIAN_POINT('Ctrl Pts',(-4.90564478570231,7.6385000069372,6.7520407912943));
#30452=CARTESIAN_POINT('Ctrl Pts',(-6.42157239285113,7.51150000693718,4.66554544007142));
#30453=CARTESIAN_POINT('Ctrl Pts',(-7.93749999999997,7.38450000693723,2.57905008884871));
#30454=CARTESIAN_POINT('Ctrl Pts',(-7.93749999999999,7.2575000069372,-5.55111512312578E-14));
#30455=CARTESIAN_POINT('Ctrl Pts',(-7.93750000000003,7.13050000693725,-2.57905008884871));
#30456=CARTESIAN_POINT('Ctrl Pts',(-6.42157239285113,7.00350000693733,-4.66554544007153));
#30457=CARTESIAN_POINT('Ctrl Pts',(-4.90564478570231,6.87650000693734,-6.7520407912943));
#30458=CARTESIAN_POINT('Ctrl Pts',(-2.45282239285116,6.74950000693719,-7.54901109809286));
#30459=CARTESIAN_POINT('Ctrl Pts',(0.,6.62250000693725,-8.34598140489129));
#30460=CARTESIAN_POINT('Ctrl Pts',(2.45282239285116,6.49550000693722,-7.54901109809286));
#30461=CARTESIAN_POINT('Ctrl Pts',(4.90564478570226,6.36850000693716,-6.7520407912943));
#30462=CARTESIAN_POINT('Ctrl Pts',(6.42157239285107,6.24150000693724,-4.66554544007153));
#30463=CARTESIAN_POINT('Ctrl Pts',(7.93749999999991,6.11450000693724,-2.57905008884871));
#30464=CARTESIAN_POINT('Ctrl Pts',(7.93749999999993,5.98750000693721,0.));
#30465=CARTESIAN_POINT('Ctrl Pts',(7.93750000000009,5.86050000693721,2.57905008884871));
#30466=CARTESIAN_POINT('Ctrl Pts',(6.42157239285118,5.73350000693723,4.66554544007147));
#30467=CARTESIAN_POINT('Ctrl Pts',(4.90564478570226,5.60650000693724,6.7520407912943));
#30468=CARTESIAN_POINT('Ctrl Pts',(2.45282239285116,5.4795000069372,7.54901109809281));
#30469=CARTESIAN_POINT('Ctrl Pts',(0.,5.35250000693721,8.34598140489129));
#30470=CARTESIAN_POINT('Ctrl Pts',(-2.45282239285111,5.22550000693722,7.54901109809281));
#30471=CARTESIAN_POINT('Ctrl Pts',(-4.90564478570231,5.09850000693718,6.7520407912943));
#30472=CARTESIAN_POINT('Ctrl Pts',(-6.42157239285113,4.97150000693714,4.66554544007147));
#30473=CARTESIAN_POINT('Ctrl Pts',(-7.93749999999997,4.8445000069372,2.57905008884871));
#30474=CARTESIAN_POINT('Ctrl Pts',(-7.93750000000004,4.71750000693721,0.));
#30475=CARTESIAN_POINT('Ctrl Pts',(-7.93749999999997,4.59050000693723,-2.57905008884871));
#30476=CARTESIAN_POINT('Ctrl Pts',(-6.42157239285118,4.46350000693724,-4.66554544007147));
#30477=CARTESIAN_POINT('Ctrl Pts',(-4.90564478570231,4.33650000693731,-6.7520407912943));
#30478=CARTESIAN_POINT('Ctrl Pts',(-2.45282239285116,4.20950000693721,-7.54901109809281));
#30479=CARTESIAN_POINT('Ctrl Pts',(0.,4.08250000693722,-8.34598140489129));
#30480=CARTESIAN_POINT('Ctrl Pts',(2.45282239285116,3.95550000693728,-7.54901109809281));
#30481=CARTESIAN_POINT('Ctrl Pts',(4.90564478570237,3.82850000693731,-6.7520407912943));
#30482=CARTESIAN_POINT('Ctrl Pts',(6.42157239285118,3.7015000069372,-4.66554544007147));
#30483=CARTESIAN_POINT('Ctrl Pts',(7.93750000000003,3.57450000693722,-2.57905008884871));
#30484=CARTESIAN_POINT('Ctrl Pts',(7.93750000000004,3.44750000693711,0.));
#30485=CARTESIAN_POINT('Ctrl Pts',(7.93750000000003,3.32050000693719,2.57905008884871));
#30486=CARTESIAN_POINT('Ctrl Pts',(6.42157239285113,3.19350000693719,4.66554544007147));
#30487=CARTESIAN_POINT('Ctrl Pts',(4.90564478570226,3.06650000693721,6.7520407912943));
#30488=CARTESIAN_POINT('Ctrl Pts',(2.45282239285111,2.93950000693721,7.54901109809281));
#30489=CARTESIAN_POINT('Ctrl Pts',(5.83678785436452E-14,2.81250000693712,
8.34598140489129));
#30490=CARTESIAN_POINT('Ctrl Pts',(-2.45282239285116,2.68550000693712,7.54901109809281));
#30491=CARTESIAN_POINT('Ctrl Pts',(-4.9056447857022,2.55850000693721,6.7520407912943));
#30492=CARTESIAN_POINT('Ctrl Pts',(-6.42157239285113,2.4315000069372,4.66554544007147));
#30493=CARTESIAN_POINT('Ctrl Pts',(-7.93750000000003,2.30450000693723,2.57905008884871));
#30494=CARTESIAN_POINT('Ctrl Pts',(-7.9375000000001,2.17750000693717,0.));
#30495=CARTESIAN_POINT('Ctrl Pts',(-7.93749999999997,2.05050000693714,-2.57905008884871));
#30496=CARTESIAN_POINT('Ctrl Pts',(-6.42157239285118,1.9235000069372,-4.66554544007147));
#30497=CARTESIAN_POINT('Ctrl Pts',(-4.90564478570231,1.79650000693723,-6.7520407912943));
#30498=CARTESIAN_POINT('Ctrl Pts',(-2.45282239285116,1.66950000693722,-7.54901109809281));
#30499=CARTESIAN_POINT('Ctrl Pts',(1.1673575708729E-13,1.54250000693726,
-8.34598140489129));
#30500=CARTESIAN_POINT('Ctrl Pts',(2.45282239285116,1.41550000693724,-7.54901109809281));
#30501=CARTESIAN_POINT('Ctrl Pts',(4.90564478570231,1.28850000693722,-6.7520407912943));
#30502=CARTESIAN_POINT('Ctrl Pts',(6.42157239285113,1.16150000693732,-4.66554544007147));
#30503=CARTESIAN_POINT('Ctrl Pts',(7.93750000000003,1.03450000693719,-2.57905008884871));
#30504=CARTESIAN_POINT('Ctrl Pts',(7.93749999999999,0.907500006937234,0.));
#30505=CARTESIAN_POINT('Ctrl Pts',(7.93749999999991,0.780500006937337,2.57905008884871));
#30506=CARTESIAN_POINT('Ctrl Pts',(6.42157239285113,0.653500006937147,4.66554544007147));
#30507=CARTESIAN_POINT('Ctrl Pts',(4.90564478570237,0.52650000693713,6.7520407912943));
#30508=CARTESIAN_POINT('Ctrl Pts',(2.45282239285122,0.399500006937226,7.54901109809281));
#30509=CARTESIAN_POINT('Ctrl Pts',(1.1673575708729E-13,0.272500006937273,
8.34598140489129));
#30510=CARTESIAN_POINT('Ctrl Pts',(-2.45282239285116,0.145500006937194,
7.54901109809281));
#30511=CARTESIAN_POINT('Ctrl Pts',(-4.90564478570231,0.0185000069371835,
6.7520407912943));
#30512=CARTESIAN_POINT('Ctrl Pts',(-6.42157239285118,-0.108499993062727,
4.66554544007147));
#30513=CARTESIAN_POINT('Ctrl Pts',(-7.93750000000003,-0.23549999306279,
2.57905008884871));
#30514=CARTESIAN_POINT('Ctrl Pts',(-7.9375000000001,-0.362499993062759,
0.));
#30515=CARTESIAN_POINT('Ctrl Pts',(-7.93749999999997,-0.489499993062763,
-2.57905008884871));
#30516=CARTESIAN_POINT('Ctrl Pts',(-6.42157239285124,-0.616499993062791,
-4.66554544007147));
#30517=CARTESIAN_POINT('Ctrl Pts',(-4.90564478570231,-0.743499993062678,
-6.7520407912943));
#30518=CARTESIAN_POINT('Ctrl Pts',(-2.45282239285105,-0.870499993062768,
-7.54901109809281));
#30519=CARTESIAN_POINT('Ctrl Pts',(0.,-0.997499993062768,-8.34598140489129));
#30520=CARTESIAN_POINT('Ctrl Pts',(2.45282239285116,-1.1244999930628,-7.54901109809281));
#30521=CARTESIAN_POINT('Ctrl Pts',(4.9056447857022,-1.2514999930628,-6.7520407912943));
#30522=CARTESIAN_POINT('Ctrl Pts',(6.42157239285113,-1.37849999306278,-4.66554544007147));
#30523=CARTESIAN_POINT('Ctrl Pts',(7.93750000000009,-1.50549999306283,-2.57905008884871));
#30524=CARTESIAN_POINT('Ctrl Pts',(7.93749999999999,-1.6324999930627,0.));
#30525=CARTESIAN_POINT('Ctrl Pts',(7.93750000000003,-1.75949999306275,2.57905008884871));
#30526=CARTESIAN_POINT('Ctrl Pts',(6.42157239285113,-1.88649999306278,4.66554544007147));
#30527=CARTESIAN_POINT('Ctrl Pts',(4.90564478570226,-2.01349999306266,6.7520407912943));
#30528=CARTESIAN_POINT('Ctrl Pts',(2.45282239285116,-2.14049999306282,7.54901109809281));
#30529=CARTESIAN_POINT('Ctrl Pts',(1.68453823965979,-2.18027950899489,7.79864175176826));
#30530=CARTESIAN_POINT('Ctrl Pts',(0.88171591555705,-2.22184731082934,7.88837646757896));
#30531=CARTESIAN_POINT('Ctrl Pts',(-6.56268467749999,15.6712500034686,-5.55111512312578E-14));
#30532=CARTESIAN_POINT('Ctrl Pts',(-6.56268467749997,15.5442500034686,-2.13234551188562));
#30533=CARTESIAN_POINT('Ctrl Pts',(-5.30932343282153,15.4172500034686,-3.85744926888038));
#30534=CARTESIAN_POINT('Ctrl Pts',(-4.05596218814312,15.2902500034686,-5.58255302587488));
#30535=CARTESIAN_POINT('Ctrl Pts',(-2.0279810940716,15.1632500034686,-6.24148402692676));
#30536=CARTESIAN_POINT('Ctrl Pts',(0.,15.0362500034687,-6.90041502797853));
#30537=CARTESIAN_POINT('Ctrl Pts',(2.0279810940716,14.9092500034685,-6.24148402692676));
#30538=CARTESIAN_POINT('Ctrl Pts',(4.05596218814312,14.7822500034687,-5.58255302587488));
#30539=CARTESIAN_POINT('Ctrl Pts',(5.30932343282159,14.6552500034686,-3.85744926888038));
#30540=CARTESIAN_POINT('Ctrl Pts',(6.56268467750003,14.5282500034687,-2.13234551188562));
#30541=CARTESIAN_POINT('Ctrl Pts',(6.56268467749999,14.4012500034687,-5.55111512312578E-14));
#30542=CARTESIAN_POINT('Ctrl Pts',(6.56268467750003,14.2742500034686,2.13234551188562));
#30543=CARTESIAN_POINT('Ctrl Pts',(5.30932343282153,14.1472500034686,3.85744926888026));
#30544=CARTESIAN_POINT('Ctrl Pts',(4.05596218814312,14.0202500034686,5.58255302587488));
#30545=CARTESIAN_POINT('Ctrl Pts',(2.0279810940716,13.8932500034686,6.24148402692665));
#30546=CARTESIAN_POINT('Ctrl Pts',(0.,13.7662500034686,6.90041502797853));
#30547=CARTESIAN_POINT('Ctrl Pts',(-2.02798109407165,13.6392500034685,6.24148402692665));
#30548=CARTESIAN_POINT('Ctrl Pts',(-4.05596218814318,13.5122500034686,5.58255302587488));
#30549=CARTESIAN_POINT('Ctrl Pts',(-5.30932343282153,13.3852500034687,3.85744926888026));
#30550=CARTESIAN_POINT('Ctrl Pts',(-6.56268467750003,13.2582500034686,2.13234551188562));
#30551=CARTESIAN_POINT('Ctrl Pts',(-6.56268467749999,13.1312500034686,-5.55111512312578E-14));
#30552=CARTESIAN_POINT('Ctrl Pts',(-6.56268467749997,13.0042500034686,-2.13234551188562));
#30553=CARTESIAN_POINT('Ctrl Pts',(-5.30932343282153,12.8772500034686,-3.85744926888038));
#30554=CARTESIAN_POINT('Ctrl Pts',(-4.05596218814312,12.7502500034686,-5.58255302587488));
#30555=CARTESIAN_POINT('Ctrl Pts',(-2.0279810940716,12.6232500034686,-6.24148402692676));
#30556=CARTESIAN_POINT('Ctrl Pts',(0.,12.4962500034686,-6.90041502797853));
#30557=CARTESIAN_POINT('Ctrl Pts',(2.0279810940716,12.3692500034686,-6.24148402692676));
#30558=CARTESIAN_POINT('Ctrl Pts',(4.05596218814318,12.2422500034686,-5.58255302587488));
#30559=CARTESIAN_POINT('Ctrl Pts',(5.30932343282159,12.1152500034687,-3.85744926888038));
#30560=CARTESIAN_POINT('Ctrl Pts',(6.56268467749997,11.9882500034686,-2.13234551188562));
#30561=CARTESIAN_POINT('Ctrl Pts',(6.56268467749999,11.8612500034686,-5.55111512312578E-14));
#30562=CARTESIAN_POINT('Ctrl Pts',(6.56268467750003,11.7342500034686,2.13234551188562));
#30563=CARTESIAN_POINT('Ctrl Pts',(5.30932343282153,11.6072500034686,3.85744926888026));
#30564=CARTESIAN_POINT('Ctrl Pts',(4.05596218814324,11.4802500034687,5.58255302587488));
#30565=CARTESIAN_POINT('Ctrl Pts',(2.02798109407154,11.3532500034686,6.24148402692665));
#30566=CARTESIAN_POINT('Ctrl Pts',(1.1673575708729E-13,11.2262500034686,
6.90041502797853));
#30567=CARTESIAN_POINT('Ctrl Pts',(-2.02798109407154,11.0992500034686,6.24148402692665));
#30568=CARTESIAN_POINT('Ctrl Pts',(-4.05596218814306,10.9722500034686,5.58255302587488));
#30569=CARTESIAN_POINT('Ctrl Pts',(-5.30932343282153,10.8452500034686,3.85744926888026));
#30570=CARTESIAN_POINT('Ctrl Pts',(-6.56268467750003,10.7182500034686,2.13234551188562));
#30571=CARTESIAN_POINT('Ctrl Pts',(-6.56268467749999,10.5912500034687,-5.55111512312578E-14));
#30572=CARTESIAN_POINT('Ctrl Pts',(-6.56268467749997,10.4642500034686,-2.13234551188562));
#30573=CARTESIAN_POINT('Ctrl Pts',(-5.30932343282159,10.3372500034685,-3.85744926888038));
#30574=CARTESIAN_POINT('Ctrl Pts',(-4.05596218814318,10.2102500034686,-5.58255302587488));
#30575=CARTESIAN_POINT('Ctrl Pts',(-2.0279810940716,10.0832500034686,-6.24148402692676));
#30576=CARTESIAN_POINT('Ctrl Pts',(1.1673575708729E-13,9.95625000346861,
-6.90041502797853));
#30577=CARTESIAN_POINT('Ctrl Pts',(2.0279810940716,9.82925000346868,-6.24148402692676));
#30578=CARTESIAN_POINT('Ctrl Pts',(4.05596218814306,9.70225000346858,-5.58255302587488));
#30579=CARTESIAN_POINT('Ctrl Pts',(5.30932343282153,9.57525000346865,-3.85744926888038));
#30580=CARTESIAN_POINT('Ctrl Pts',(6.56268467749997,9.4482500034686,-2.13234551188562));
#30581=CARTESIAN_POINT('Ctrl Pts',(6.56268467749999,9.32125000346862,-5.55111512312578E-14));
#30582=CARTESIAN_POINT('Ctrl Pts',(6.56268467750003,9.19425000346858,2.13234551188562));
#30583=CARTESIAN_POINT('Ctrl Pts',(5.30932343282153,9.06725000346864,3.85744926888026));
#30584=CARTESIAN_POINT('Ctrl Pts',(4.05596218814318,8.94025000346872,5.58255302587488));
#30585=CARTESIAN_POINT('Ctrl Pts',(2.02798109407165,8.81325000346872,6.24148402692665));
#30586=CARTESIAN_POINT('Ctrl Pts',(1.1673575708729E-13,8.68625000346869,
6.90041502797853));
#30587=CARTESIAN_POINT('Ctrl Pts',(-2.0279810940716,8.55925000346869,6.24148402692665));
#30588=CARTESIAN_POINT('Ctrl Pts',(-4.05596218814306,8.4322500034686,5.58255302587488));
#30589=CARTESIAN_POINT('Ctrl Pts',(-5.30932343282159,8.3052500034686,3.85744926888026));
#30590=CARTESIAN_POINT('Ctrl Pts',(-6.56268467749991,8.17825000346862,2.13234551188562));
#30591=CARTESIAN_POINT('Ctrl Pts',(-6.56268467749999,8.05125000346868,-5.55111512312578E-14));
#30592=CARTESIAN_POINT('Ctrl Pts',(-6.56268467749997,7.92425000346871,-2.13234551188562));
#30593=CARTESIAN_POINT('Ctrl Pts',(-5.30932343282159,7.79725000346859,-3.85744926888038));
#30594=CARTESIAN_POINT('Ctrl Pts',(-4.05596218814306,7.67025000346873,-5.58255302587488));
#30595=CARTESIAN_POINT('Ctrl Pts',(-2.0279810940716,7.54325000346862,-6.24148402692676));
#30596=CARTESIAN_POINT('Ctrl Pts',(-1.1673575708729E-13,7.41625000346859,
-6.90041502797853));
#30597=CARTESIAN_POINT('Ctrl Pts',(2.02798109407154,7.28925000346869,-6.24148402692676));
#30598=CARTESIAN_POINT('Ctrl Pts',(4.05596218814318,7.16225000346861,-5.58255302587488));
#30599=CARTESIAN_POINT('Ctrl Pts',(5.30932343282153,7.03525000346861,-3.85744926888038));
#30600=CARTESIAN_POINT('Ctrl Pts',(6.56268467750008,6.90825000346864,-2.13234551188562));
#30601=CARTESIAN_POINT('Ctrl Pts',(6.56268467749999,6.78125000346857,-5.55111512312578E-14));
#30602=CARTESIAN_POINT('Ctrl Pts',(6.56268467750003,6.65425000346861,2.13234551188562));
#30603=CARTESIAN_POINT('Ctrl Pts',(5.30932343282148,6.5272500034686,3.85744926888026));
#30604=CARTESIAN_POINT('Ctrl Pts',(4.05596218814318,6.40025000346864,5.58255302587488));
#30605=CARTESIAN_POINT('Ctrl Pts',(2.0279810940716,6.27325000346862,6.24148402692665));
#30606=CARTESIAN_POINT('Ctrl Pts',(-1.1673575708729E-13,6.14625000346872,
6.90041502797853));
#30607=CARTESIAN_POINT('Ctrl Pts',(-2.0279810940716,6.01925000346865,6.2414840269267));
#30608=CARTESIAN_POINT('Ctrl Pts',(-4.05596218814324,5.89225000346851,5.58255302587488));
#30609=CARTESIAN_POINT('Ctrl Pts',(-5.30932343282159,5.76525000346861,3.85744926888032));
#30610=CARTESIAN_POINT('Ctrl Pts',(-6.56268467750003,5.63825000346866,2.13234551188562));
#30611=CARTESIAN_POINT('Ctrl Pts',(-6.56268467750004,5.51125000346864,0.));
#30612=CARTESIAN_POINT('Ctrl Pts',(-6.56268467749997,5.38425000346863,-2.13234551188562));
#30613=CARTESIAN_POINT('Ctrl Pts',(-5.30932343282148,5.25725000346872,-3.85744926888032));
#30614=CARTESIAN_POINT('Ctrl Pts',(-4.05596218814318,5.13025000346865,-5.58255302587488));
#30615=CARTESIAN_POINT('Ctrl Pts',(-2.02798109407165,5.00325000346863,-6.2414840269267));
#30616=CARTESIAN_POINT('Ctrl Pts',(0.,4.87625000346868,-6.90041502797853));
#30617=CARTESIAN_POINT('Ctrl Pts',(2.02798109407154,4.7492500034686,-6.2414840269267));
#30618=CARTESIAN_POINT('Ctrl Pts',(4.05596218814312,4.62225000346859,-5.58255302587488));
#30619=CARTESIAN_POINT('Ctrl Pts',(5.30932343282148,4.49525000346862,-3.85744926888032));
#30620=CARTESIAN_POINT('Ctrl Pts',(6.56268467750008,4.36825000346862,-2.13234551188562));
#30621=CARTESIAN_POINT('Ctrl Pts',(6.5626846775001,4.24125000346864,0.));
#30622=CARTESIAN_POINT('Ctrl Pts',(6.56268467750003,4.1142500034687,2.13234551188562));
#30623=CARTESIAN_POINT('Ctrl Pts',(5.30932343282148,3.98725000346861,3.85744926888032));
#30624=CARTESIAN_POINT('Ctrl Pts',(4.05596218814318,3.86025000346873,5.58255302587488));
#30625=CARTESIAN_POINT('Ctrl Pts',(2.0279810940716,3.73325000346858,6.2414840269267));
#30626=CARTESIAN_POINT('Ctrl Pts',(0.,3.60625000346864,6.90041502797853));
#30627=CARTESIAN_POINT('Ctrl Pts',(-2.0279810940716,3.4792500034686,6.2414840269267));
#30628=CARTESIAN_POINT('Ctrl Pts',(-4.05596218814312,3.35225000346861,5.58255302587488));
#30629=CARTESIAN_POINT('Ctrl Pts',(-5.30932343282159,3.22525000346852,3.85744926888032));
#30630=CARTESIAN_POINT('Ctrl Pts',(-6.56268467749991,3.09825000346869,2.13234551188562));
#30631=CARTESIAN_POINT('Ctrl Pts',(-6.5626846775001,2.9712500034686,0.));
#30632=CARTESIAN_POINT('Ctrl Pts',(-6.56268467750003,2.8442500034686,-2.13234551188562));
#30633=CARTESIAN_POINT('Ctrl Pts',(-5.30932343282148,2.71725000346862,-3.85744926888032));
#30634=CARTESIAN_POINT('Ctrl Pts',(-4.05596218814306,2.59025000346863,-5.58255302587488));
#30635=CARTESIAN_POINT('Ctrl Pts',(-2.02798109407165,2.46325000346864,-6.2414840269267));
#30636=CARTESIAN_POINT('Ctrl Pts',(0.,2.3362500034686,-6.90041502797853));
#30637=CARTESIAN_POINT('Ctrl Pts',(2.02798109407165,2.20925000346861,-6.2414840269267));
#30638=CARTESIAN_POINT('Ctrl Pts',(4.05596218814312,2.08225000346851,-5.58255302587488));
#30639=CARTESIAN_POINT('Ctrl Pts',(5.30932343282148,1.95525000346858,-3.85744926888032));
#30640=CARTESIAN_POINT('Ctrl Pts',(6.56268467749997,1.82825000346865,-2.13234551188562));
#30641=CARTESIAN_POINT('Ctrl Pts',(6.56268467750004,1.7012500034686,0.));
#30642=CARTESIAN_POINT('Ctrl Pts',(6.56268467750014,1.57425000346862,2.13234551188562));
#30643=CARTESIAN_POINT('Ctrl Pts',(5.30932343282148,1.44725000346863,3.85744926888032));
#30644=CARTESIAN_POINT('Ctrl Pts',(4.05596218814318,1.32025000346859,5.58255302587488));
#30645=CARTESIAN_POINT('Ctrl Pts',(2.0279810940716,1.19325000346859,6.2414840269267));
#30646=CARTESIAN_POINT('Ctrl Pts',(0.,1.06625000346873,6.90041502797853));
#30647=CARTESIAN_POINT('Ctrl Pts',(-2.0279810940716,0.939250003468617,6.2414840269267));
#30648=CARTESIAN_POINT('Ctrl Pts',(-4.05596218814312,0.81225000346864,5.58255302587488));
#30649=CARTESIAN_POINT('Ctrl Pts',(-5.30932343282148,0.685250003468529,
3.85744926888032));
#30650=CARTESIAN_POINT('Ctrl Pts',(-6.56268467749997,0.558250003468608,
2.13234551188562));
#30651=CARTESIAN_POINT('Ctrl Pts',(-6.5626846775001,0.431250003468608,0.));
#30652=CARTESIAN_POINT('Ctrl Pts',(-6.56268467750003,0.304250003468635,
-2.13234551188562));
#30653=CARTESIAN_POINT('Ctrl Pts',(-5.30932343282153,0.177250003468632,
-3.85744926888032));
#30654=CARTESIAN_POINT('Ctrl Pts',(-4.05596218814312,0.0502500034686033,
-5.58255302587488));
#30655=CARTESIAN_POINT('Ctrl Pts',(-2.02798109407154,-0.0767499965314,-6.2414840269267));
#30656=CARTESIAN_POINT('Ctrl Pts',(0.,-0.203749996531312,-6.90041502797853));
#30657=CARTESIAN_POINT('Ctrl Pts',(2.0279810940716,-0.330749996531432,-6.2414840269267));
#30658=CARTESIAN_POINT('Ctrl Pts',(4.05596218814312,-0.457749996531285,
-5.58255302587488));
#30659=CARTESIAN_POINT('Ctrl Pts',(5.30932343282148,-0.584749996531464,
-3.85744926888032));
#30660=CARTESIAN_POINT('Ctrl Pts',(6.56268467750003,-0.711749996531317,
-2.13234551188562));
#30661=CARTESIAN_POINT('Ctrl Pts',(6.56268467750004,-0.838749996531385,
0.));
#30662=CARTESIAN_POINT('Ctrl Pts',(6.56268467749997,-0.96574999653129,2.13234551188562));
#30663=CARTESIAN_POINT('Ctrl Pts',(5.30932343282159,-1.09274999653142,3.85744926888032));
#30664=CARTESIAN_POINT('Ctrl Pts',(4.05596218814312,-1.21974999653144,5.58255302587488));
#30665=CARTESIAN_POINT('Ctrl Pts',(2.0279810940716,-1.34674999653139,6.2414840269267));
#30666=CARTESIAN_POINT('Ctrl Pts',(1.39276765909645,-1.38652951246359,6.44787738326189));
#30667=CARTESIAN_POINT('Ctrl Pts',(0.728998239865705,-1.42809731429797,
6.52206959044185));
#30668=CARTESIAN_POINT('Origin',(-9.68966956780948,-5.53100000000001,0.));
#30669=CARTESIAN_POINT('Origin',(100.349250287849,58.0000000000003,-5.55111512312578E-14));
#30670=CARTESIAN_POINT('',(0.,0.,0.));
#30671=CARTESIAN_POINT('Origin',(-34.9249999999999,0.,0.));
#30672=CARTESIAN_POINT('',(-2.413,-2.04055548261129E-15,-16.6624));
#30673=CARTESIAN_POINT('Origin',(-2.413,0.,0.));
#30674=CARTESIAN_POINT('',(0.,-2.04055548261129E-15,-16.6624));
#30675=CARTESIAN_POINT('',(-34.9249999999999,-2.04055548261129E-15,-16.6624));
#30676=CARTESIAN_POINT('Origin',(0.,0.,0.));
#30677=CARTESIAN_POINT('Origin',(-34.9249999999999,0.,0.));
#30678=CARTESIAN_POINT('',(0.,-1.02027774130564E-15,-8.3312));
#30679=CARTESIAN_POINT('Origin',(0.,0.,0.));
#30680=CARTESIAN_POINT('',(-2.413,-1.02027774130564E-15,-8.3312));
#30681=CARTESIAN_POINT('',(-34.9249999999999,-1.02027774130564E-15,-8.3312));
#30682=CARTESIAN_POINT('Origin',(-2.413,0.,0.));
#30683=CARTESIAN_POINT('Origin',(0.,8.3312,0.));
#30684=CARTESIAN_POINT('Origin',(-2.413,16.6624,0.));
#30685=CARTESIAN_POINT('',(0.,0.,0.));
#30686=CARTESIAN_POINT('',(0.793085967014081,7.99999999999934,1.30104260698261E-14));
#30687=CARTESIAN_POINT('',(-340.039729762984,0.,-155.0625));
#30688=CARTESIAN_POINT('',(-340.039729762984,-6.66133814775094E-13,183.2151));
#30689=CARTESIAN_POINT('',(286.9375,-36.9375,-136.5724));
#30690=CARTESIAN_POINT('',(-340.039729762983,-8.46545056276682E-13,138.4509));
#30691=CARTESIAN_POINT('',(286.9375,-36.9375,171.7));
#30692=CARTESIAN_POINT('',(286.9375,10.4625,163.7625));
#30693=CARTESIAN_POINT('',(-340.039729762984,0.,155.0625));
#30694=CARTESIAN_POINT('',(286.9375,-36.9375,178.55));
#30695=CARTESIAN_POINT('',(286.9375,-36.9375,-178.55));
#30696=CARTESIAN_POINT('',(-340.039729762983,-7.21644966006352E-13,-183.2151));
#30697=CARTESIAN_POINT('',(286.9375,-36.9375,136.5724));
#30698=CARTESIAN_POINT('',(-340.039729762984,0.,-138.4509));
#30699=CARTESIAN_POINT('',(286.9375,-36.9375,-195.1616));
#30700=CARTESIAN_POINT('',(286.9375,-36.9375,195.1616));
#30701=CARTESIAN_POINT('',(286.9375,-36.9375,-155.825));
#30702=CARTESIAN_POINT('',(286.9375,10.4625,163.7625));
#30703=CARTESIAN_POINT('',(286.114886973474,9.95528524259992,-163.7625));
#30704=CARTESIAN_POINT('',(286.114886973474,9.95528524259992,-163.7625));
#30705=CARTESIAN_POINT('',(0.,0.,0.));
#30706=CARTESIAN_POINT('Origin',(400.,-277.5,15.875));
#30707=CARTESIAN_POINT('',(400.,-277.5,0.));
#30708=CARTESIAN_POINT('',(400.,277.5,0.));
#30709=CARTESIAN_POINT('',(400.,-277.5,0.));
#30710=CARTESIAN_POINT('',(400.,277.5,15.875));
#30711=CARTESIAN_POINT('',(400.,277.5,15.875));
#30712=CARTESIAN_POINT('',(400.,-277.5,15.875));
#30713=CARTESIAN_POINT('',(400.,-277.5,15.875));
#30714=CARTESIAN_POINT('',(400.,-277.5,15.875));
#30715=CARTESIAN_POINT('Origin',(-400.,277.5,15.875));
#30716=CARTESIAN_POINT('',(-400.,277.5,0.));
#30717=CARTESIAN_POINT('',(-400.,277.5,0.));
#30718=CARTESIAN_POINT('',(-400.,277.5,15.875));
#30719=CARTESIAN_POINT('',(-400.,277.5,15.875));
#30720=CARTESIAN_POINT('',(-400.,277.5,15.875));
#30721=CARTESIAN_POINT('Origin',(-400.,-277.5,15.875));
#30722=CARTESIAN_POINT('',(-400.,-277.5,0.));
#30723=CARTESIAN_POINT('',(-400.,-277.5,0.));
#30724=CARTESIAN_POINT('',(-400.,-277.5,15.875));
#30725=CARTESIAN_POINT('',(-400.,-277.5,15.875));
#30726=CARTESIAN_POINT('',(-400.,-277.5,15.875));
#30727=CARTESIAN_POINT('Origin',(-400.,-277.5,15.875));
#30728=CARTESIAN_POINT('',(-400.,-277.5,0.));
#30729=CARTESIAN_POINT('',(-400.,-277.5,15.875));
#30730=CARTESIAN_POINT('Origin',(0.,0.,15.875));
#30731=CARTESIAN_POINT('Origin',(0.,0.,0.));
#30732=CARTESIAN_POINT('Origin',(412.7,-0.499999999999945,-407.52));
#30733=CARTESIAN_POINT('',(412.7,-0.49999999999995,-447.52));
#30734=CARTESIAN_POINT('Origin',(412.7,-0.499999999999945,-407.52));
#30735=CARTESIAN_POINT('',(400.,-0.49999999999995,-447.52));
#30736=CARTESIAN_POINT('',(412.7,-0.49999999999995,-447.52));
#30737=CARTESIAN_POINT('Origin',(400.,-0.499999999999945,-407.52));
#30738=CARTESIAN_POINT('Origin',(412.7,277.5,-647.52));
#30739=CARTESIAN_POINT('',(412.7,277.5,0.));
#30740=CARTESIAN_POINT('',(412.7,-282.5,0.));
#30741=CARTESIAN_POINT('',(412.7,-282.5,0.));
#30742=CARTESIAN_POINT('',(412.7,-532.5,-433.));
#30743=CARTESIAN_POINT('',(412.7,-532.5,-433.));
#30744=CARTESIAN_POINT('',(412.7,23.5000000000001,-754.));
#30745=CARTESIAN_POINT('',(412.7,23.5000000000001,-754.));
#30746=CARTESIAN_POINT('',(412.7,230.764157791864,-588.861999240546));
#30747=CARTESIAN_POINT('',(412.7,230.764157791864,-588.861999240546));
#30748=CARTESIAN_POINT('',(412.7,277.5,-572.52));
#30749=CARTESIAN_POINT('Origin',(412.7,277.5,-647.52));
#30750=CARTESIAN_POINT('',(412.7,277.5,0.));
#30751=CARTESIAN_POINT('Origin',(400.,277.5,-647.52));
#30752=CARTESIAN_POINT('',(400.,277.5,0.));
#30753=CARTESIAN_POINT('',(400.,-282.5,0.));
#30754=CARTESIAN_POINT('',(400.,-282.5,0.));
#30755=CARTESIAN_POINT('',(400.,277.5,-572.52));
#30756=CARTESIAN_POINT('',(400.,277.5,0.));
#30757=CARTESIAN_POINT('',(400.,230.764157791864,-588.861999240546));
#30758=CARTESIAN_POINT('Origin',(400.,277.5,-647.52));
#30759=CARTESIAN_POINT('',(400.,23.5000000000001,-754.));
#30760=CARTESIAN_POINT('',(400.,230.764157791864,-588.861999240546));
#30761=CARTESIAN_POINT('',(400.,-532.5,-433.));
#30762=CARTESIAN_POINT('',(400.,23.5000000000001,-754.));
#30763=CARTESIAN_POINT('',(400.,-532.5,-433.));
#30764=CARTESIAN_POINT('Origin',(412.7,-282.5,0.));
#30765=CARTESIAN_POINT('',(412.7,-282.5,0.));
#30766=CARTESIAN_POINT('',(412.7,277.5,0.));
#30767=CARTESIAN_POINT('Origin',(412.7,-532.5,-433.));
#30768=CARTESIAN_POINT('',(412.7,-532.5,-433.));
#30769=CARTESIAN_POINT('Origin',(412.7,23.5000000000001,-754.));
#30770=CARTESIAN_POINT('',(412.7,23.5000000000001,-754.));
#30771=CARTESIAN_POINT('Origin',(412.7,230.764157791864,-588.861999240546));
#30772=CARTESIAN_POINT('',(412.7,230.764157791864,-588.861999240546));
#30773=CARTESIAN_POINT('Origin',(412.7,277.5,-647.52));
#30774=CARTESIAN_POINT('',(412.7,277.5,-572.52));
#30775=CARTESIAN_POINT('Origin',(412.7,277.5,0.));
#30776=CARTESIAN_POINT('Origin',(-412.7,-0.499999999999945,-407.52));
#30777=CARTESIAN_POINT('',(-412.7,-0.49999999999994,-447.52));
#30778=CARTESIAN_POINT('Origin',(-412.7,-0.499999999999945,-407.52));
#30779=CARTESIAN_POINT('',(-400.,-0.49999999999994,-447.52));
#30780=CARTESIAN_POINT('',(-412.7,-0.49999999999994,-447.52));
#30781=CARTESIAN_POINT('Origin',(-400.,-0.499999999999945,-407.52));
#30782=CARTESIAN_POINT('Origin',(-412.7,277.5,-647.52));
#30783=CARTESIAN_POINT('',(-412.7,277.5,0.));
#30784=CARTESIAN_POINT('',(-412.7,-282.5,0.));
#30785=CARTESIAN_POINT('',(-412.7,-282.5,0.));
#30786=CARTESIAN_POINT('',(-412.7,277.5,-572.52));
#30787=CARTESIAN_POINT('',(-412.7,277.5,0.));
#30788=CARTESIAN_POINT('',(-412.7,230.764157791864,-588.861999240546));
#30789=CARTESIAN_POINT('Origin',(-412.7,277.5,-647.52));
#30790=CARTESIAN_POINT('',(-412.7,23.5000000000001,-754.));
#30791=CARTESIAN_POINT('',(-412.7,230.764157791864,-588.861999240546));
#30792=CARTESIAN_POINT('',(-412.7,-532.5,-433.));
#30793=CARTESIAN_POINT('',(-412.7,23.5000000000001,-754.));
#30794=CARTESIAN_POINT('',(-412.7,-532.5,-433.));
#30795=CARTESIAN_POINT('Origin',(-400.,277.5,-647.52));
#30796=CARTESIAN_POINT('',(-400.,277.5,0.));
#30797=CARTESIAN_POINT('',(-400.,-282.5,0.));
#30798=CARTESIAN_POINT('',(-400.,-282.5,0.));
#30799=CARTESIAN_POINT('',(-400.,-532.5,-433.));
#30800=CARTESIAN_POINT('',(-400.,-532.5,-433.));
#30801=CARTESIAN_POINT('',(-400.,23.5000000000001,-754.));
#30802=CARTESIAN_POINT('',(-400.,23.5000000000001,-754.));
#30803=CARTESIAN_POINT('',(-400.,230.764157791864,-588.861999240546));
#30804=CARTESIAN_POINT('',(-400.,230.764157791864,-588.861999240546));
#30805=CARTESIAN_POINT('',(-400.,277.5,-572.52));
#30806=CARTESIAN_POINT('Origin',(-400.,277.5,-647.52));
#30807=CARTESIAN_POINT('',(-400.,277.5,0.));
#30808=CARTESIAN_POINT('Origin',(-412.7,-282.5,0.));
#30809=CARTESIAN_POINT('',(-412.7,277.5,0.));
#30810=CARTESIAN_POINT('',(-412.7,-282.5,0.));
#30811=CARTESIAN_POINT('Origin',(-412.7,-532.5,-433.));
#30812=CARTESIAN_POINT('',(-412.7,-532.5,-433.));
#30813=CARTESIAN_POINT('Origin',(-412.7,23.5000000000001,-754.));
#30814=CARTESIAN_POINT('',(-412.7,23.5000000000001,-754.));
#30815=CARTESIAN_POINT('Origin',(-412.7,230.764157791864,-588.861999240546));
#30816=CARTESIAN_POINT('',(-412.7,230.764157791864,-588.861999240546));
#30817=CARTESIAN_POINT('Origin',(-412.7,277.5,-647.52));
#30818=CARTESIAN_POINT('',(-412.7,277.5,-572.52));
#30819=CARTESIAN_POINT('Origin',(-412.7,277.5,0.));
#30820=CARTESIAN_POINT('Origin',(300.,-4.50064876413007,-752.498777568804));
#30821=CARTESIAN_POINT('',(300.,3.2936208412868,-756.998706603586));
#30822=CARTESIAN_POINT('Origin',(300.,-4.50064876413007,-752.498777568804));
#30823=CARTESIAN_POINT('',(300.,9.64352070147921,-746.000126160387));
#30824=CARTESIAN_POINT('',(300.,3.2936208412868,-756.998706603586));
#30825=CARTESIAN_POINT('Origin',(300.,1.84925109606238,-741.500197125605));
#30826=CARTESIAN_POINT('Origin',(150.,-4.50064876412913,-752.498777568804));
#30827=CARTESIAN_POINT('',(150.,3.29362084128775,-756.998706603587));
#30828=CARTESIAN_POINT('Origin',(150.,-4.50064876412913,-752.498777568804));
#30829=CARTESIAN_POINT('',(150.,9.64352070148016,-746.000126160387));
#30830=CARTESIAN_POINT('',(150.,3.29362084128775,-756.998706603587));
#30831=CARTESIAN_POINT('Origin',(150.,1.84925109606332,-741.500197125605));
#30832=CARTESIAN_POINT('Origin',(-300.,-4.50064876412824,-752.498777568805));
#30833=CARTESIAN_POINT('',(-300.,3.29362084128862,-756.998706603587));
#30834=CARTESIAN_POINT('Origin',(-300.,-4.50064876412824,-752.498777568805));
#30835=CARTESIAN_POINT('',(-300.,9.64352070148111,-746.000126160388));
#30836=CARTESIAN_POINT('',(-300.,3.29362084128863,-756.998706603587));
#30837=CARTESIAN_POINT('Origin',(-300.,1.84925109606421,-741.500197125606));
#30838=CARTESIAN_POINT('Origin',(-150.,-4.50064876412824,-752.498777568805));
#30839=CARTESIAN_POINT('',(-150.,3.29362084128864,-756.998706603587));
#30840=CARTESIAN_POINT('Origin',(-150.,-4.50064876412824,-752.498777568805));
#30841=CARTESIAN_POINT('',(-150.,9.64352070148113,-746.000126160388));
#30842=CARTESIAN_POINT('',(-150.,3.29362084128864,-756.998706603587));
#30843=CARTESIAN_POINT('Origin',(-150.,1.84925109606421,-741.500197125606));
#30844=CARTESIAN_POINT('Origin',(0.,-4.50064876412824,-752.498777568805));
#30845=CARTESIAN_POINT('',(-1.10218211923262E-15,3.29362084128864,-756.998706603587));
#30846=CARTESIAN_POINT('Origin',(0.,-4.50064876412824,-752.498777568805));
#30847=CARTESIAN_POINT('',(-1.10218211923262E-15,9.64352070148112,-746.000126160388));
#30848=CARTESIAN_POINT('',(-1.10218211923262E-15,3.29362084128864,-756.998706603587));
#30849=CARTESIAN_POINT('Origin',(0.,1.84925109606421,-741.500197125606));
#30850=CARTESIAN_POINT('Origin',(0.,-326.963229813101,-566.328834193409));
#30851=CARTESIAN_POINT('',(400.,17.1501001398076,-764.9985804432));
#30852=CARTESIAN_POINT('',(400.,-538.849899860193,-443.9985804432));
#30853=CARTESIAN_POINT('',(400.,-538.849899860193,-443.9985804432));
#30854=CARTESIAN_POINT('',(250.,-764.017688461125,-314.000630549496));
#30855=CARTESIAN_POINT('',(250.,-764.017688461125,-314.000630549496));
#30856=CARTESIAN_POINT('',(250.,-805.587126356682,-290.001009030658));
#30857=CARTESIAN_POINT('',(250.,-805.587126356682,-290.001009030658));
#30858=CARTESIAN_POINT('',(-250.,-805.587126356682,-290.001009030658));
#30859=CARTESIAN_POINT('',(-250.,-805.587126356682,-290.001009030658));
#30860=CARTESIAN_POINT('',(-250.,-764.017688461125,-314.000630549496));
#30861=CARTESIAN_POINT('',(-250.,-764.017688461125,-314.000630549496));
#30862=CARTESIAN_POINT('',(-400.,-538.849899860193,-443.9985804432));
#30863=CARTESIAN_POINT('',(-400.,-538.849899860193,-443.9985804432));
#30864=CARTESIAN_POINT('',(-400.,17.1501001398076,-764.9985804432));
#30865=CARTESIAN_POINT('',(-400.,17.1501001398076,-764.9985804432));
#30866=CARTESIAN_POINT('',(400.,17.1501001398076,-764.9985804432));
#30867=CARTESIAN_POINT('Origin',(0.,-320.613329952909,-555.33025375021));
#30868=CARTESIAN_POINT('',(400.,23.5,-754.));
#30869=CARTESIAN_POINT('',(400.,-532.5,-433.));
#30870=CARTESIAN_POINT('',(400.,-532.5,-433.));
#30871=CARTESIAN_POINT('',(-400.,23.5,-754.));
#30872=CARTESIAN_POINT('',(400.,23.5,-754.));
#30873=CARTESIAN_POINT('',(-400.,-532.5,-433.));
#30874=CARTESIAN_POINT('',(-400.,23.5,-754.));
#30875=CARTESIAN_POINT('',(-250.,-757.667788600933,-303.002050106297));
#30876=CARTESIAN_POINT('',(-400.,-532.5,-433.));
#30877=CARTESIAN_POINT('',(-250.,-799.237226496489,-279.002428587459));
#30878=CARTESIAN_POINT('',(-250.,-757.667788600933,-303.002050106297));
#30879=CARTESIAN_POINT('',(250.,-799.237226496489,-279.002428587459));
#30880=CARTESIAN_POINT('',(-250.,-799.237226496489,-279.002428587459));
#30881=CARTESIAN_POINT('',(250.,-757.667788600933,-303.002050106297));
#30882=CARTESIAN_POINT('',(250.,-799.237226496489,-279.002428587459));
#30883=CARTESIAN_POINT('',(250.,-757.667788600933,-303.002050106297));
#30884=CARTESIAN_POINT('Origin',(400.,-538.849899860193,-443.9985804432));
#30885=CARTESIAN_POINT('',(400.,-538.849899860193,-443.9985804432));
#30886=CARTESIAN_POINT('',(400.,17.1501001398076,-764.9985804432));
#30887=CARTESIAN_POINT('Origin',(250.,-764.017688461125,-314.000630549496));
#30888=CARTESIAN_POINT('',(250.,-764.017688461125,-314.000630549496));
#30889=CARTESIAN_POINT('Origin',(250.,-805.587126356682,-290.001009030658));
#30890=CARTESIAN_POINT('',(250.,-805.587126356682,-290.001009030658));
#30891=CARTESIAN_POINT('Origin',(-250.,-805.587126356682,-290.001009030658));
#30892=CARTESIAN_POINT('',(-250.,-805.587126356682,-290.001009030658));
#30893=CARTESIAN_POINT('Origin',(-250.,-764.017688461125,-314.000630549496));
#30894=CARTESIAN_POINT('',(-250.,-764.017688461125,-314.000630549496));
#30895=CARTESIAN_POINT('Origin',(-400.,-538.849899860193,-443.9985804432));
#30896=CARTESIAN_POINT('',(-400.,-538.849899860193,-443.9985804432));
#30897=CARTESIAN_POINT('Origin',(-400.,17.1501001398076,-764.9985804432));
#30898=CARTESIAN_POINT('',(-400.,17.1501001398076,-764.9985804432));
#30899=CARTESIAN_POINT('Origin',(400.,17.1501001398076,-764.9985804432));
#30900=CARTESIAN_POINT('Origin',(411.000556942817,-537.996237603978,-429.826812462452));
#30901=CARTESIAN_POINT('',(251.582431340073,-755.289566540481,-304.368610542448));
#30902=CARTESIAN_POINT('',(400.,-532.5,-433.));
#30903=CARTESIAN_POINT('',(400.,-532.5,-433.));
#30904=CARTESIAN_POINT('',(411.000556942817,-537.996237603978,-429.826812462452));
#30905=CARTESIAN_POINT('',(411.000556942817,-537.996237603978,-429.826812462452));
#30906=CARTESIAN_POINT('',(262.58298828289,-760.785804144459,-301.195423004899));
#30907=CARTESIAN_POINT('',(411.000556942817,-537.996237603978,-429.826812462452));
#30908=CARTESIAN_POINT('',(262.58298828289,-760.785804144459,-301.195423004899));
#30909=CARTESIAN_POINT('Origin',(411.000556942817,-537.996237603978,-429.826812462452));
#30910=CARTESIAN_POINT('',(400.004719499877,-282.502358016311,0.00136137272609138));
#30911=CARTESIAN_POINT('',(400.,-532.5,-433.));
#30912=CARTESIAN_POINT('',(411.005276442694,-287.998595620289,3.17454891027458));
#30913=CARTESIAN_POINT('',(411.005276442694,-287.998595620289,3.17454891027458));
#30914=CARTESIAN_POINT('',(411.000556942817,-537.996237603978,-429.826812462452));
#30915=CARTESIAN_POINT('Origin',(411.005276442694,-287.998595620289,3.17454891027458));
#30916=CARTESIAN_POINT('',(251.58715083995,-505.291924556791,128.632750830278));
#30917=CARTESIAN_POINT('',(400.004719499877,-282.502358016311,0.00136137272609138));
#30918=CARTESIAN_POINT('',(262.587707782767,-510.788162160769,131.805938367827));
#30919=CARTESIAN_POINT('',(262.587707782767,-510.788162160769,131.805938367827));
#30920=CARTESIAN_POINT('',(411.005276442694,-287.998595620289,3.17454891027458));
#30921=CARTESIAN_POINT('Origin',(262.58298828289,-760.785804144459,-301.195423004899));
#30922=CARTESIAN_POINT('',(251.582431340073,-755.289566540481,-304.368610542448));
#30923=CARTESIAN_POINT('',(262.58298828289,-760.785804144459,-301.195423004899));
#30924=CARTESIAN_POINT('Origin',(417.015099327983,-208.354366262308,120.290920090289));
#30925=CARTESIAN_POINT('Origin',(406.014542385166,-202.85812865833,117.117732552741));
#30926=CARTESIAN_POINT('Origin',(262.7,-799.237226496489,-279.002428587459));
#30927=CARTESIAN_POINT('',(250.,-799.237226496489,-279.002428587459));
#30928=CARTESIAN_POINT('',(250.,-760.266369128196,-301.502923603794));
#30929=CARTESIAN_POINT('',(250.,-799.237226496489,-279.002428587459));
#30930=CARTESIAN_POINT('',(262.7,-760.266369128196,-301.502923603794));
#30931=CARTESIAN_POINT('',(262.7,-760.266369128196,-301.502923603794));
#30932=CARTESIAN_POINT('',(262.7,-799.237226496489,-279.002428587459));
#30933=CARTESIAN_POINT('',(262.7,-799.237226496489,-279.002428587459));
#30934=CARTESIAN_POINT('',(262.7,-799.237226496489,-279.002428587459));
#30935=CARTESIAN_POINT('Origin',(262.7,-760.266369128196,-301.502923603794));
#30936=CARTESIAN_POINT('',(250.,-510.263080007906,131.502773152548));
#30937=CARTESIAN_POINT('',(250.,-760.266369128196,-301.502923603794));
#30938=CARTESIAN_POINT('',(262.7,-510.263080007906,131.502773152548));
#30939=CARTESIAN_POINT('',(262.7,-510.263080007906,131.502773152548));
#30940=CARTESIAN_POINT('',(262.7,-760.266369128196,-301.502923603794));
#30941=CARTESIAN_POINT('Origin',(262.7,-549.2339373762,154.003268168884));
#30942=CARTESIAN_POINT('',(250.,-549.2339373762,154.003268168884));
#30943=CARTESIAN_POINT('',(250.,-549.2339373762,154.003268168884));
#30944=CARTESIAN_POINT('',(262.7,-549.2339373762,154.003268168884));
#30945=CARTESIAN_POINT('',(262.7,-549.2339373762,154.003268168884));
#30946=CARTESIAN_POINT('',(262.7,-549.2339373762,154.003268168884));
#30947=CARTESIAN_POINT('Origin',(262.7,-799.237226496489,-279.002428587459));
#30948=CARTESIAN_POINT('',(250.,-799.237226496489,-279.002428587459));
#30949=CARTESIAN_POINT('',(262.7,-799.237226496489,-279.002428587459));
#30950=CARTESIAN_POINT('Origin',(262.7,0.,0.));
#30951=CARTESIAN_POINT('Origin',(250.,0.,0.));
#30952=CARTESIAN_POINT('Origin',(249.998786597631,-501.314873870463,141.001336655876));
#30953=CARTESIAN_POINT('',(249.998666719697,-507.664953680518,130.00286010721));
#30954=CARTESIAN_POINT('',(400.,-282.5,-1.38777878078145E-14));
#30955=CARTESIAN_POINT('',(249.998666719697,-507.664953680518,130.00286010721));
#30956=CARTESIAN_POINT('',(400.000119877934,-276.149920189945,10.998476548666));
#30957=CARTESIAN_POINT('',(400.000119877934,-276.149920189945,10.998476548666));
#30958=CARTESIAN_POINT('',(249.998786597631,-501.314873870463,141.001336655876));
#30959=CARTESIAN_POINT('',(249.998786597631,-501.314873870463,141.001336655876));
#30960=CARTESIAN_POINT('',(249.998786597631,-501.314873870463,141.001336655876));
#30961=CARTESIAN_POINT('Origin',(400.000119877934,-276.149920189945,10.998476548666));
#30962=CARTESIAN_POINT('',(-399.999999928721,-282.496224269578,0.00653964733464407));
#30963=CARTESIAN_POINT('',(400.,-282.5,-1.38777878078145E-14));
#30964=CARTESIAN_POINT('',(-399.999880050787,-276.146144459522,11.0050161960007));
#30965=CARTESIAN_POINT('',(-399.999880050787,-276.146144459522,11.0050161960007));
#30966=CARTESIAN_POINT('',(400.000119877934,-276.149920189945,10.998476548666));
#30967=CARTESIAN_POINT('Origin',(-399.999880050787,-276.146144459522,11.0050161960007));
#30968=CARTESIAN_POINT('',(-250.001333258029,-507.662593849004,130.006947386795));
#30969=CARTESIAN_POINT('',(-399.999999928721,-282.496224269578,0.00653964733464407));
#30970=CARTESIAN_POINT('',(-250.001213380094,-501.312514038949,141.005423935461));
#30971=CARTESIAN_POINT('',(-250.001213380094,-501.312514038949,141.005423935461));
#30972=CARTESIAN_POINT('',(-399.999880050787,-276.146144459522,11.0050161960007));
#30973=CARTESIAN_POINT('Origin',(-250.001213380094,-501.312514038949,141.005423935461));
#30974=CARTESIAN_POINT('',(-250.001333258029,-549.231639074161,154.007249032168));
#30975=CARTESIAN_POINT('',(-250.001333258029,-507.662593849004,130.006947386795));
#30976=CARTESIAN_POINT('',(-250.001213380094,-542.881559264105,165.005725580834));
#30977=CARTESIAN_POINT('',(-250.001213380094,-542.881559264105,165.005725580834));
#30978=CARTESIAN_POINT('',(-250.001213380094,-501.312514038949,141.005423935461));
#30979=CARTESIAN_POINT('Origin',(-250.001213380094,-542.881559264105,165.005725580834));
#30980=CARTESIAN_POINT('',(249.998666719697,-549.233998905675,154.003161752583));
#30981=CARTESIAN_POINT('',(-250.001333258029,-549.231639074161,154.007249032168));
#30982=CARTESIAN_POINT('',(249.998786597631,-542.883919095619,165.001638301249));
#30983=CARTESIAN_POINT('',(249.998786597631,-542.883919095619,165.001638301249));
#30984=CARTESIAN_POINT('',(-250.001213380094,-542.881559264105,165.005725580834));
#30985=CARTESIAN_POINT('Origin',(249.998786597631,-542.883919095619,165.001638301249));
#30986=CARTESIAN_POINT('',(249.998666719697,-549.233998905675,154.003161752583));
#30987=CARTESIAN_POINT('',(249.998786597631,-542.883919095619,165.001638301249));
#30988=CARTESIAN_POINT('Origin',(-0.00121339123172574,-64.2748076383018,
-111.325366865542));
#30989=CARTESIAN_POINT('Origin',(-0.00133326916594913,-70.6248874483571,
-122.323843414208));
#30990=CARTESIAN_POINT('Origin',(296.200000000004,-734.583240701635,-141.622283996917));
#30991=CARTESIAN_POINT('',(296.200000000004,-739.083339704902,-149.416455470576));
#30992=CARTESIAN_POINT('Origin',(296.200000000004,-734.583240701635,-141.622283996917));
#30993=CARTESIAN_POINT('',(296.200000000004,-728.084897736517,-155.766595175186));
#30994=CARTESIAN_POINT('',(296.200000000004,-739.083339704902,-149.416455470576));
#30995=CARTESIAN_POINT('Origin',(296.200000000004,-723.58479873325,-147.972423701528));
#30996=CARTESIAN_POINT('Origin',(296.200000000002,-635.581062629759,29.8494884235731));
#30997=CARTESIAN_POINT('',(296.200000000002,-640.081161633026,22.0553169499145));
#30998=CARTESIAN_POINT('Origin',(296.200000000002,-635.581062629759,29.8494884235731));
#30999=CARTESIAN_POINT('',(296.200000000002,-629.082719664641,15.7051772453043));
#31000=CARTESIAN_POINT('',(296.200000000002,-640.081161633026,22.0553169499145));
#31001=CARTESIAN_POINT('Origin',(296.200000000002,-624.582620661374,23.4993487189629));
#31002=CARTESIAN_POINT('Origin',(296.2,-536.578884557882,201.321260844064));
#31003=CARTESIAN_POINT('',(296.2,-541.078983561149,193.527089370405));
#31004=CARTESIAN_POINT('Origin',(296.2,-536.578884557882,201.321260844064));
#31005=CARTESIAN_POINT('',(296.2,-530.080541592764,187.176949665795));
#31006=CARTESIAN_POINT('',(296.2,-541.078983561149,193.527089370405));
#31007=CARTESIAN_POINT('Origin',(296.2,-525.580442589497,194.971121139453));
#31008=CARTESIAN_POINT('Origin',(0.,-489.60420247788,282.681410206628));
#31009=CARTESIAN_POINT('',(262.7,-521.578554546992,227.301832422926));
#31010=CARTESIAN_POINT('',(262.7,-816.585044761169,-283.649408628031));
#31011=CARTESIAN_POINT('',(262.7,-521.578554546992,227.301832422926));
#31012=CARTESIAN_POINT('',(326.2,-816.585044761169,-283.649408628031));
#31013=CARTESIAN_POINT('',(262.7,-816.585044761169,-283.649408628031));
#31014=CARTESIAN_POINT('',(326.2,-521.578554546992,227.301832422926));
#31015=CARTESIAN_POINT('',(326.2,-521.578554546992,227.301832422926));
#31016=CARTESIAN_POINT('',(262.7,-521.578554546992,227.301832422926));
#31017=CARTESIAN_POINT('Origin',(0.,-478.605760509495,276.331270502017));
#31018=CARTESIAN_POINT('',(262.7,-510.580112578607,220.951692718316));
#31019=CARTESIAN_POINT('',(262.7,-805.586602792784,-289.999548332641));
#31020=CARTESIAN_POINT('',(262.7,-510.580112578607,220.951692718316));
#31021=CARTESIAN_POINT('',(326.2,-510.580112578607,220.951692718316));
#31022=CARTESIAN_POINT('',(262.7,-510.580112578607,220.951692718316));
#31023=CARTESIAN_POINT('',(326.2,-805.586602792784,-289.999548332641));
#31024=CARTESIAN_POINT('',(326.2,-510.580112578607,220.951692718316));
#31025=CARTESIAN_POINT('',(262.7,-805.586602792784,-289.999548332641));
#31026=CARTESIAN_POINT('Origin',(262.7,-521.578554546992,227.301832422926));
#31027=CARTESIAN_POINT('',(262.7,-816.585044761169,-283.649408628031));
#31028=CARTESIAN_POINT('',(262.7,-521.578554546992,227.301832422926));
#31029=CARTESIAN_POINT('Origin',(262.7,-816.585044761169,-283.649408628031));
#31030=CARTESIAN_POINT('',(326.2,-816.585044761169,-283.649408628031));
#31031=CARTESIAN_POINT('Origin',(326.2,-521.578554546992,227.301832422926));
#31032=CARTESIAN_POINT('',(326.2,-521.578554546992,227.301832422926));
#31033=CARTESIAN_POINT('Origin',(262.7,-521.578554546992,227.301832422926));
#31034=CARTESIAN_POINT('Origin',(98.6978247534365,-537.131180039572,200.368985977147));
#31035=CARTESIAN_POINT('',(107.697824753303,-537.131222484398,200.36901048309));
#31036=CARTESIAN_POINT('Origin',(98.6978247534365,-537.131180039572,200.368985977147));
#31037=CARTESIAN_POINT('',(107.69789391365,-526.132745935405,194.018930672846));
#31038=CARTESIAN_POINT('',(107.697824753303,-537.131222484398,200.36901048309));
#31039=CARTESIAN_POINT('Origin',(98.6978939137833,-526.132703490579,194.018906166903));
#31040=CARTESIAN_POINT('Origin',(-99.3021752436275,-537.130246253392,200.368446846407));
#31041=CARTESIAN_POINT('',(-90.302175243761,-537.130288698218,200.368471352349));
#31042=CARTESIAN_POINT('Origin',(-99.3021752436275,-537.130246253392,200.368446846407));
#31043=CARTESIAN_POINT('',(-90.3021060834143,-526.131812149225,194.018391542105));
#31044=CARTESIAN_POINT('',(-90.302175243761,-537.130288698218,200.368471352349));
#31045=CARTESIAN_POINT('Origin',(-99.3021060832809,-526.131769704399,194.018367036163));
#31046=CARTESIAN_POINT('Origin',(-297.302175240692,-537.129312467211,200.367907715666));
#31047=CARTESIAN_POINT('',(-288.302175240825,-537.129354912038,200.367932221609));
#31048=CARTESIAN_POINT('Origin',(-297.302175240692,-537.129312467211,200.367907715666));
#31049=CARTESIAN_POINT('',(-288.302106080479,-526.130878363045,194.017852411365));
#31050=CARTESIAN_POINT('',(-288.302175240825,-537.129354912038,200.367932221609));
#31051=CARTESIAN_POINT('Origin',(-297.302106080345,-526.130835918218,194.017827905422));
#31052=CARTESIAN_POINT('Origin',(-391.249472490554,-685.230730806452,-56.1479980020244));
#31053=CARTESIAN_POINT('',(-327.302175240247,-553.87938150779,171.356096549133));
#31054=CARTESIAN_POINT('',(262.697824751005,-553.882164001966,171.357703049819));
#31055=CARTESIAN_POINT('',(-327.302175240247,-553.87938150779,171.356096549133));
#31056=CARTESIAN_POINT('',(262.697824751005,-522.131764950275,226.350085795599));
#31057=CARTESIAN_POINT('',(262.697824751005,-553.882164001966,171.357703049819));
#31058=CARTESIAN_POINT('',(-327.302175240247,-522.128982456099,226.348479294913));
#31059=CARTESIAN_POINT('',(-327.302175240247,-522.128982456099,226.348479294913));
#31060=CARTESIAN_POINT('',(-327.302175240247,-553.87938150779,171.356096549133));
#31061=CARTESIAN_POINT('Origin',(-391.249403330208,-674.232254257459,-62.4980778122685));
#31062=CARTESIAN_POINT('',(-327.3021060799,-542.880904958797,165.006016738889));
#31063=CARTESIAN_POINT('',(262.697893911352,-542.883687452973,165.007623239575));
#31064=CARTESIAN_POINT('',(-327.3021060799,-542.880904958797,165.006016738889));
#31065=CARTESIAN_POINT('',(-327.3021060799,-511.130505907106,219.998399484669));
#31066=CARTESIAN_POINT('',(-327.3021060799,-542.880904958797,165.006016738889));
#31067=CARTESIAN_POINT('',(262.697893911351,-511.133288401282,220.000005985355));
#31068=CARTESIAN_POINT('',(-327.3021060799,-511.130505907106,219.998399484669));
#31069=CARTESIAN_POINT('',(262.697893911352,-542.883687452973,165.007623239575));
#31070=CARTESIAN_POINT('Origin',(-327.302175240247,-553.87938150779,171.356096549133));
#31071=CARTESIAN_POINT('',(262.697824751005,-553.882164001966,171.357703049819));
#31072=CARTESIAN_POINT('',(-327.302175240247,-553.87938150779,171.356096549133));
#31073=CARTESIAN_POINT('Origin',(262.697824751005,-553.882164001966,171.357703049819));
#31074=CARTESIAN_POINT('',(262.697824751005,-522.131764950275,226.350085795599));
#31075=CARTESIAN_POINT('Origin',(-327.302175240247,-522.128982456099,226.348479294913));
#31076=CARTESIAN_POINT('',(-327.302175240247,-522.128982456099,226.348479294913));
#31077=CARTESIAN_POINT('Origin',(-327.302175240247,-553.87938150779,171.356096549133));
#31078=CARTESIAN_POINT('Origin',(-296.201333258033,-635.883508821549,29.3278015002441));
#31079=CARTESIAN_POINT('',(-296.201333258033,-631.383494707935,37.122021985788));
#31080=CARTESIAN_POINT('Origin',(-296.201333258033,-635.883508821549,29.3278015002441));
#31081=CARTESIAN_POINT('',(-296.201333258033,-620.384983578334,30.7720020699101));
#31082=CARTESIAN_POINT('',(-296.201333258033,-631.383494707935,37.122021985788));
#31083=CARTESIAN_POINT('Origin',(-296.201333258033,-624.884997691948,22.9777815843661));
#31084=CARTESIAN_POINT('Origin',(-296.201333258031,-734.883819321062,-142.145049181723));
#31085=CARTESIAN_POINT('',(-296.201333258031,-730.383805207448,-134.350828696179));
#31086=CARTESIAN_POINT('Origin',(-296.201333258031,-734.883819321062,-142.145049181723));
#31087=CARTESIAN_POINT('',(-296.201333258031,-719.385294077847,-140.700848612057));
#31088=CARTESIAN_POINT('',(-296.201333258031,-730.383805207448,-134.350828696179));
#31089=CARTESIAN_POINT('Origin',(-296.201333258031,-723.885308191461,-148.4950690976));
#31090=CARTESIAN_POINT('Origin',(-296.201333258029,-833.884129820575,-313.617899863689));
#31091=CARTESIAN_POINT('',(-296.201333258029,-829.384115706961,-305.823679378145));
#31092=CARTESIAN_POINT('Origin',(-296.201333258029,-833.884129820575,-313.617899863689));
#31093=CARTESIAN_POINT('',(-296.201333258029,-818.38560457736,-312.173699294023));
#31094=CARTESIAN_POINT('',(-296.201333258029,-829.384115706961,-305.823679378145));
#31095=CARTESIAN_POINT('Origin',(-296.201333258029,-822.885618690974,-319.967919779567));
#31096=CARTESIAN_POINT('Origin',(-0.00133325802852044,-880.857925772416,
-394.978560841159));
#31097=CARTESIAN_POINT('',(-262.701333258028,-848.884176865956,-339.598634815502));
#31098=CARTESIAN_POINT('',(-262.701333258029,-553.883251640134,171.355819236822));
#31099=CARTESIAN_POINT('',(-262.701333258028,-848.884176865956,-339.598634815502));
#31100=CARTESIAN_POINT('',(-326.201333258029,-553.883251640134,171.355819236822));
#31101=CARTESIAN_POINT('',(-262.701333258029,-553.883251640134,171.355819236822));
#31102=CARTESIAN_POINT('',(-326.201333258029,-848.884176865956,-339.598634815502));
#31103=CARTESIAN_POINT('',(-326.201333258029,-848.884176865956,-339.598634815502));
#31104=CARTESIAN_POINT('',(-262.701333258028,-848.884176865956,-339.598634815502));
#31105=CARTESIAN_POINT('Origin',(-0.00133325802852079,-869.859414642815,
-401.328580757037));
#31106=CARTESIAN_POINT('',(-262.701333258028,-837.885665736355,-345.94865473138));
#31107=CARTESIAN_POINT('',(-262.701333258029,-542.884740510533,165.005799320944));
#31108=CARTESIAN_POINT('',(-262.701333258028,-837.885665736355,-345.94865473138));
#31109=CARTESIAN_POINT('',(-326.201333258029,-837.885665736355,-345.94865473138));
#31110=CARTESIAN_POINT('',(-262.701333258028,-837.885665736355,-345.94865473138));
#31111=CARTESIAN_POINT('',(-326.201333258029,-542.884740510533,165.005799320944));
#31112=CARTESIAN_POINT('',(-326.201333258029,-837.885665736355,-345.94865473138));
#31113=CARTESIAN_POINT('',(-262.701333258029,-542.884740510533,165.005799320944));
#31114=CARTESIAN_POINT('Origin',(-262.701333258028,-848.884176865956,-339.598634815502));
#31115=CARTESIAN_POINT('',(-262.701333258029,-553.883251640134,171.355819236822));
#31116=CARTESIAN_POINT('',(-262.701333258028,-848.884176865956,-339.598634815502));
#31117=CARTESIAN_POINT('Origin',(-262.701333258029,-553.883251640134,171.355819236822));
#31118=CARTESIAN_POINT('',(-326.201333258029,-553.883251640134,171.355819236822));
#31119=CARTESIAN_POINT('Origin',(-326.201333258029,-848.884176865956,-339.598634815502));
#31120=CARTESIAN_POINT('',(-326.201333258029,-848.884176865956,-339.598634815502));
#31121=CARTESIAN_POINT('Origin',(-262.701333258028,-848.884176865956,-339.598634815502));
#31122=CARTESIAN_POINT('Origin',(-98.6991580114631,-833.335569483613,-312.663468473821));
#31123=CARTESIAN_POINT('',(-107.69915801133,-833.335611928439,-312.663443967878));
#31124=CARTESIAN_POINT('Origin',(-98.6991580114631,-833.335569483613,-312.663468473821));
#31125=CARTESIAN_POINT('',(-107.699227171676,-822.337135379446,-319.013523778122));
#31126=CARTESIAN_POINT('',(-107.69915801133,-833.335611928439,-312.663443967878));
#31127=CARTESIAN_POINT('Origin',(-98.6992271718098,-822.33709293462,-319.013548284065));
#31128=CARTESIAN_POINT('Origin',(99.300841985601,-833.334635697429,-312.664007604555));
#31129=CARTESIAN_POINT('',(90.3008419857345,-833.334678142255,-312.663983098613));
#31130=CARTESIAN_POINT('Origin',(99.300841985601,-833.334635697429,-312.664007604555));
#31131=CARTESIAN_POINT('',(90.3007728253878,-822.336201593263,-319.014062908857));
#31132=CARTESIAN_POINT('',(90.3008419857345,-833.334678142255,-312.663983098613));
#31133=CARTESIAN_POINT('Origin',(99.3007728252544,-822.336159148436,-319.014087414799));
#31134=CARTESIAN_POINT('Origin',(297.300841982665,-833.333701911245,-312.66454673529));
#31135=CARTESIAN_POINT('',(288.300841982799,-833.333744356072,-312.664522229347));
#31136=CARTESIAN_POINT('Origin',(297.300841982665,-833.333701911245,-312.66454673529));
#31137=CARTESIAN_POINT('',(288.300772822452,-822.335267807078,-319.014602039592));
#31138=CARTESIAN_POINT('',(288.300841982799,-833.333744356072,-312.664522229347));
#31139=CARTESIAN_POINT('Origin',(297.300772822319,-822.335225362252,-319.014626545534));
#31140=CARTESIAN_POINT('Origin',(391.248139232526,-685.231397443842,-56.1491526325048));
#31141=CARTESIAN_POINT('',(327.30084198222,-816.583349905157,-283.652898941708));
#31142=CARTESIAN_POINT('',(-262.699158009032,-816.586132399338,-283.651292441029));
#31143=CARTESIAN_POINT('',(327.30084198222,-816.583349905157,-283.652898941708));
#31144=CARTESIAN_POINT('',(-262.699158009031,-848.336531451029,-338.643675186809));
#31145=CARTESIAN_POINT('',(-262.699158009032,-816.586132399338,-283.651292441029));
#31146=CARTESIAN_POINT('',(327.300841982221,-848.333748956848,-338.645281687488));
#31147=CARTESIAN_POINT('',(327.300841982221,-848.333748956848,-338.645281687488));
#31148=CARTESIAN_POINT('',(327.30084198222,-816.583349905157,-283.652898941708));
#31149=CARTESIAN_POINT('Origin',(391.248070072179,-674.232920894849,-62.4992324427489));
#31150=CARTESIAN_POINT('',(327.300772821873,-805.584873356164,-290.002978751952));
#31151=CARTESIAN_POINT('',(-262.699227169378,-805.587655850345,-290.001372251273));
#31152=CARTESIAN_POINT('',(327.300772821873,-805.584873356164,-290.002978751952));
#31153=CARTESIAN_POINT('',(327.300772821874,-837.335272407855,-344.995361497732));
#31154=CARTESIAN_POINT('',(327.300772821873,-805.584873356164,-290.002978751952));
#31155=CARTESIAN_POINT('',(-262.699227169378,-837.338054902036,-344.993754997053));
#31156=CARTESIAN_POINT('',(327.300772821874,-837.335272407855,-344.995361497732));
#31157=CARTESIAN_POINT('',(-262.699227169378,-805.587655850345,-290.001372251273));
#31158=CARTESIAN_POINT('Origin',(327.30084198222,-816.583349905157,-283.652898941708));
#31159=CARTESIAN_POINT('',(-262.699158009032,-816.586132399338,-283.651292441029));
#31160=CARTESIAN_POINT('',(327.30084198222,-816.583349905157,-283.652898941708));
#31161=CARTESIAN_POINT('Origin',(-262.699158009032,-816.586132399338,-283.651292441029));
#31162=CARTESIAN_POINT('',(-262.699158009031,-848.336531451029,-338.643675186809));
#31163=CARTESIAN_POINT('Origin',(327.300841982221,-848.333748956848,-338.645281687488));
#31164=CARTESIAN_POINT('',(327.300841982221,-848.333748956848,-338.645281687488));
#31165=CARTESIAN_POINT('Origin',(327.30084198222,-816.583349905157,-283.652898941708));
#31166=CARTESIAN_POINT('Origin',(-411.000556942817,-537.996237603978,-429.826812462452));
#31167=CARTESIAN_POINT('',(-251.582431340073,-755.289566540481,-304.368610542448));
#31168=CARTESIAN_POINT('',(-400.,-532.5,-433.));
#31169=CARTESIAN_POINT('',(-400.,-532.5,-433.));
#31170=CARTESIAN_POINT('',(-262.58298828289,-760.785804144459,-301.195423004899));
#31171=CARTESIAN_POINT('',(-262.58298828289,-760.785804144459,-301.195423004899));
#31172=CARTESIAN_POINT('',(-411.000556942817,-537.996237603978,-429.826812462452));
#31173=CARTESIAN_POINT('',(-411.000556942817,-537.996237603978,-429.826812462452));
#31174=CARTESIAN_POINT('',(-411.000556942817,-537.996237603978,-429.826812462452));
#31175=CARTESIAN_POINT('Origin',(-411.000556942817,-537.996237603978,-429.826812462452));
#31176=CARTESIAN_POINT('',(-400.004719499877,-282.502358016311,0.00136137272609138));
#31177=CARTESIAN_POINT('',(-400.,-532.5,-433.));
#31178=CARTESIAN_POINT('',(-411.005276442694,-287.998595620289,3.17454891027458));
#31179=CARTESIAN_POINT('',(-411.000556942817,-537.996237603978,-429.826812462452));
#31180=CARTESIAN_POINT('',(-411.005276442694,-287.998595620289,3.17454891027458));
#31181=CARTESIAN_POINT('Origin',(-411.005276442694,-287.998595620289,3.17454891027458));
#31182=CARTESIAN_POINT('',(-251.58715083995,-505.291924556791,128.632750830278));
#31183=CARTESIAN_POINT('',(-400.004719499877,-282.502358016311,0.00136137272609138));
#31184=CARTESIAN_POINT('',(-262.587707782767,-510.788162160769,131.805938367827));
#31185=CARTESIAN_POINT('',(-411.005276442694,-287.998595620289,3.17454891027458));
#31186=CARTESIAN_POINT('',(-262.587707782767,-510.788162160769,131.805938367827));
#31187=CARTESIAN_POINT('Origin',(-262.58298828289,-760.785804144459,-301.195423004899));
#31188=CARTESIAN_POINT('',(-251.582431340073,-755.289566540481,-304.368610542448));
#31189=CARTESIAN_POINT('',(-262.58298828289,-760.785804144459,-301.195423004899));
#31190=CARTESIAN_POINT('Origin',(-417.015099327983,-208.354366262308,120.290920090289));
#31191=CARTESIAN_POINT('Origin',(-406.014542385166,-202.85812865833,117.117732552741));
#31192=CARTESIAN_POINT('Origin',(-262.7,-799.237226496489,-279.002428587459));
#31193=CARTESIAN_POINT('',(-250.,-799.237226496489,-279.002428587459));
#31194=CARTESIAN_POINT('',(-250.,-760.266369128196,-301.502923603794));
#31195=CARTESIAN_POINT('',(-250.,-799.237226496489,-279.002428587459));
#31196=CARTESIAN_POINT('',(-262.7,-799.237226496489,-279.002428587459));
#31197=CARTESIAN_POINT('',(-262.7,-799.237226496489,-279.002428587459));
#31198=CARTESIAN_POINT('',(-262.7,-760.266369128196,-301.502923603794));
#31199=CARTESIAN_POINT('',(-262.7,-799.237226496489,-279.002428587459));
#31200=CARTESIAN_POINT('',(-262.7,-760.266369128196,-301.502923603794));
#31201=CARTESIAN_POINT('Origin',(-262.7,-760.266369128196,-301.502923603794));
#31202=CARTESIAN_POINT('',(-250.,-510.263080007906,131.502773152548));
#31203=CARTESIAN_POINT('',(-250.,-760.266369128196,-301.502923603794));
#31204=CARTESIAN_POINT('',(-262.7,-510.263080007906,131.502773152548));
#31205=CARTESIAN_POINT('',(-262.7,-760.266369128196,-301.502923603794));
#31206=CARTESIAN_POINT('',(-262.7,-510.263080007906,131.502773152548));
#31207=CARTESIAN_POINT('Origin',(-262.7,-549.2339373762,154.003268168884));
#31208=CARTESIAN_POINT('',(-250.,-549.2339373762,154.003268168884));
#31209=CARTESIAN_POINT('',(-250.,-549.2339373762,154.003268168884));
#31210=CARTESIAN_POINT('',(-262.7,-549.2339373762,154.003268168884));
#31211=CARTESIAN_POINT('',(-262.7,-549.2339373762,154.003268168884));
#31212=CARTESIAN_POINT('',(-262.7,-549.2339373762,154.003268168884));
#31213=CARTESIAN_POINT('Origin',(-262.7,-799.237226496489,-279.002428587459));
#31214=CARTESIAN_POINT('',(-250.,-799.237226496489,-279.002428587459));
#31215=CARTESIAN_POINT('',(-262.7,-799.237226496489,-279.002428587459));
#31216=CARTESIAN_POINT('Origin',(-262.7,0.,0.));
#31217=CARTESIAN_POINT('Origin',(-250.,0.,0.));
#31218=CARTESIAN_POINT('Origin',(463.499333370986,293.375,15.8749999999999));
#31219=CARTESIAN_POINT('',(463.499333370986,277.5,15.8749999999999));
#31220=CARTESIAN_POINT('',(463.499333370986,277.5,66.6749999999998));
#31221=CARTESIAN_POINT('',(463.499333370986,277.5,15.8749999999999));
#31222=CARTESIAN_POINT('',(463.499333370986,293.375,15.8749999999999));
#31223=CARTESIAN_POINT('',(463.499333370986,293.375,15.8749999999999));
#31224=CARTESIAN_POINT('',(463.499333370986,293.375,66.6749999999998));
#31225=CARTESIAN_POINT('',(463.499333370986,293.375,15.8749999999999));
#31226=CARTESIAN_POINT('',(463.499333370986,293.375,66.6749999999998));
#31227=CARTESIAN_POINT('Origin',(463.499333370986,293.375,15.8749999999999));
#31228=CARTESIAN_POINT('',(-463.500666629014,277.5,15.8749999999999));
#31229=CARTESIAN_POINT('',(463.499333370986,277.5,15.8749999999999));
#31230=CARTESIAN_POINT('',(-463.500666629014,293.375,15.8749999999999));
#31231=CARTESIAN_POINT('',(-463.500666629014,293.375,15.8749999999999));
#31232=CARTESIAN_POINT('',(463.499333370986,293.375,15.8749999999999));
#31233=CARTESIAN_POINT('Origin',(-463.500666629014,293.375,15.8749999999999));
#31234=CARTESIAN_POINT('',(-463.500666629014,277.5,66.6749999999998));
#31235=CARTESIAN_POINT('',(-463.500666629014,277.5,15.8749999999999));
#31236=CARTESIAN_POINT('',(-463.500666629014,293.375,66.6749999999998));
#31237=CARTESIAN_POINT('',(-463.500666629014,293.375,66.6749999999998));
#31238=CARTESIAN_POINT('',(-463.500666629014,293.375,15.8749999999999));
#31239=CARTESIAN_POINT('Origin',(463.499333370986,293.375,66.6749999999998));
#31240=CARTESIAN_POINT('',(463.499333370986,277.5,66.6749999999998));
#31241=CARTESIAN_POINT('',(463.499333370986,293.375,66.6749999999998));
#31242=CARTESIAN_POINT('Origin',(0.,293.375,0.));
#31243=CARTESIAN_POINT('Origin',(0.,277.5,0.));
#31244=CARTESIAN_POINT('Origin',(412.7,277.5,-453.125));
#31245=CARTESIAN_POINT('',(412.7,293.375,-453.125));
#31246=CARTESIAN_POINT('',(412.7,293.375,15.8749999999999));
#31247=CARTESIAN_POINT('',(412.7,293.375,-453.125));
#31248=CARTESIAN_POINT('',(412.7,277.5,-453.125));
#31249=CARTESIAN_POINT('',(412.7,277.5,-453.125));
#31250=CARTESIAN_POINT('',(412.7,277.5,15.8749999999999));
#31251=CARTESIAN_POINT('',(412.7,277.5,-453.125));
#31252=CARTESIAN_POINT('',(412.7,277.5,15.8749999999999));
#31253=CARTESIAN_POINT('Origin',(412.7,277.5,-453.125));
#31254=CARTESIAN_POINT('',(463.499333370981,293.375,-453.125));
#31255=CARTESIAN_POINT('',(412.7,293.375,-453.125));
#31256=CARTESIAN_POINT('',(463.499333370981,277.5,-453.125));
#31257=CARTESIAN_POINT('',(463.499333370981,277.5,-453.125));
#31258=CARTESIAN_POINT('',(412.7,277.5,-453.125));
#31259=CARTESIAN_POINT('Origin',(463.499333370981,277.5,-453.125));
#31260=CARTESIAN_POINT('',(463.499333370986,293.375,15.8749999999999));
#31261=CARTESIAN_POINT('',(463.499333370981,293.375,-453.125));
#31262=CARTESIAN_POINT('',(463.499333370986,277.5,15.8749999999999));
#31263=CARTESIAN_POINT('',(463.499333370986,277.5,15.8749999999999));
#31264=CARTESIAN_POINT('',(463.499333370981,277.5,-453.125));
#31265=CARTESIAN_POINT('Origin',(412.7,277.5,15.8749999999999));
#31266=CARTESIAN_POINT('',(412.7,293.375,15.8749999999999));
#31267=CARTESIAN_POINT('',(412.7,277.5,15.8749999999999));
#31268=CARTESIAN_POINT('Origin',(0.,277.5,0.));
#31269=CARTESIAN_POINT('Origin',(0.,293.375,0.));
#31270=CARTESIAN_POINT('Origin',(-412.7,277.5,-453.125));
#31271=CARTESIAN_POINT('',(-412.7,293.375,-453.125));
#31272=CARTESIAN_POINT('',(-412.7,293.375,15.8749999999999));
#31273=CARTESIAN_POINT('',(-412.7,293.375,-453.125));
#31274=CARTESIAN_POINT('',(-412.7,277.5,15.8749999999999));
#31275=CARTESIAN_POINT('',(-412.7,277.5,15.8749999999999));
#31276=CARTESIAN_POINT('',(-412.7,277.5,-453.125));
#31277=CARTESIAN_POINT('',(-412.7,277.5,-453.125));
#31278=CARTESIAN_POINT('',(-412.7,277.5,-453.125));
#31279=CARTESIAN_POINT('Origin',(-412.7,277.5,-453.125));
#31280=CARTESIAN_POINT('',(-463.499333370981,293.375,-453.125));
#31281=CARTESIAN_POINT('',(-412.7,293.375,-453.125));
#31282=CARTESIAN_POINT('',(-463.499333370981,277.5,-453.125));
#31283=CARTESIAN_POINT('',(-412.7,277.5,-453.125));
#31284=CARTESIAN_POINT('',(-463.499333370981,277.5,-453.125));
#31285=CARTESIAN_POINT('Origin',(-463.499333370981,277.5,-453.125));
#31286=CARTESIAN_POINT('',(-463.499333370986,293.375,15.8749999999999));
#31287=CARTESIAN_POINT('',(-463.499333370981,293.375,-453.125));
#31288=CARTESIAN_POINT('',(-463.499333370986,277.5,15.8749999999999));
#31289=CARTESIAN_POINT('',(-463.499333370981,277.5,-453.125));
#31290=CARTESIAN_POINT('',(-463.499333370986,277.5,15.8749999999999));
#31291=CARTESIAN_POINT('Origin',(-412.7,277.5,15.8749999999999));
#31292=CARTESIAN_POINT('',(-412.7,293.375,15.8749999999999));
#31293=CARTESIAN_POINT('',(-412.7,277.5,15.8749999999999));
#31294=CARTESIAN_POINT('Origin',(0.,277.5,0.));
#31295=CARTESIAN_POINT('Origin',(0.,293.375,0.));
#31296=CARTESIAN_POINT('Origin',(579.199999999996,191.625,-54.1249999999996));
#31297=CARTESIAN_POINT('',(579.199999999996,191.625,-63.1249999999996));
#31298=CARTESIAN_POINT('Origin',(579.199999999996,191.625,-54.1249999999996));
#31299=CARTESIAN_POINT('',(579.199999999996,207.5,-63.1249999999996));
#31300=CARTESIAN_POINT('',(579.199999999996,191.625,-63.1249999999996));
#31301=CARTESIAN_POINT('Origin',(579.199999999996,207.5,-54.1249999999996));
#31302=CARTESIAN_POINT('Origin',(579.199999999998,191.625,-174.125));
#31303=CARTESIAN_POINT('',(579.199999999998,191.625,-183.125));
#31304=CARTESIAN_POINT('Origin',(579.199999999998,191.625,-174.125));
#31305=CARTESIAN_POINT('',(579.199999999998,207.5,-183.125));
#31306=CARTESIAN_POINT('',(579.199999999998,191.625,-183.125));
#31307=CARTESIAN_POINT('Origin',(579.199999999998,207.5,-174.125));
#31308=CARTESIAN_POINT('Origin',(579.199999999999,191.625,-294.125));
#31309=CARTESIAN_POINT('',(579.199999999999,191.625,-303.125));
#31310=CARTESIAN_POINT('Origin',(579.199999999999,191.625,-294.125));
#31311=CARTESIAN_POINT('',(579.199999999999,207.5,-303.125));
#31312=CARTESIAN_POINT('',(579.199999999999,191.625,-303.125));
#31313=CARTESIAN_POINT('Origin',(579.199999999999,207.5,-294.125));
#31314=CARTESIAN_POINT('Origin',(579.2,191.625,-414.125));
#31315=CARTESIAN_POINT('',(579.2,191.625,-423.125));
#31316=CARTESIAN_POINT('Origin',(579.2,191.625,-414.125));
#31317=CARTESIAN_POINT('',(579.2,207.5,-423.125));
#31318=CARTESIAN_POINT('',(579.2,191.625,-423.125));
#31319=CARTESIAN_POINT('Origin',(579.2,207.5,-414.125));
#31320=CARTESIAN_POINT('Origin',(0.,191.625,0.));
#31321=CARTESIAN_POINT('',(412.7,191.625,15.8749999999999));
#31322=CARTESIAN_POINT('',(412.7,191.625,-453.125));
#31323=CARTESIAN_POINT('',(412.7,191.625,-453.125));
#31324=CARTESIAN_POINT('',(595.7,191.625,-453.125));
#31325=CARTESIAN_POINT('',(412.7,191.625,-453.125));
#31326=CARTESIAN_POINT('',(595.7,191.625,15.8749999999999));
#31327=CARTESIAN_POINT('',(595.7,191.625,-453.125));
#31328=CARTESIAN_POINT('',(412.7,191.625,15.8749999999999));
#31329=CARTESIAN_POINT('Origin',(0.,207.5,0.));
#31330=CARTESIAN_POINT('',(412.7,207.5,15.8749999999999));
#31331=CARTESIAN_POINT('',(412.7,207.5,-453.125));
#31332=CARTESIAN_POINT('',(412.7,207.5,-453.125));
#31333=CARTESIAN_POINT('',(595.7,207.5,15.8749999999999));
#31334=CARTESIAN_POINT('',(412.7,207.5,15.8749999999999));
#31335=CARTESIAN_POINT('',(595.7,207.5,-453.125));
#31336=CARTESIAN_POINT('',(595.7,207.5,-453.125));
#31337=CARTESIAN_POINT('',(412.7,207.5,-453.125));
#31338=CARTESIAN_POINT('Origin',(412.7,191.625,-453.125));
#31339=CARTESIAN_POINT('',(412.7,191.625,-453.125));
#31340=CARTESIAN_POINT('',(412.7,191.625,15.8749999999999));
#31341=CARTESIAN_POINT('Origin',(412.7,191.625,-453.125));
#31342=CARTESIAN_POINT('',(595.7,191.625,-453.125));
#31343=CARTESIAN_POINT('Origin',(595.7,191.625,-453.125));
#31344=CARTESIAN_POINT('',(595.7,191.625,15.8749999999999));
#31345=CARTESIAN_POINT('Origin',(412.7,191.625,15.8749999999999));
#31346=CARTESIAN_POINT('Origin',(-265.5,207.5,135.874999999997));
#31347=CARTESIAN_POINT('',(-265.5,207.5,144.874999999997));
#31348=CARTESIAN_POINT('Origin',(-265.5,207.5,135.874999999997));
#31349=CARTESIAN_POINT('',(-265.5,191.625,144.874999999997));
#31350=CARTESIAN_POINT('',(-265.5,207.5,144.874999999997));
#31351=CARTESIAN_POINT('Origin',(-265.5,191.625,135.874999999997));
#31352=CARTESIAN_POINT('Origin',(-88.5,207.5,135.874999999999));
#31353=CARTESIAN_POINT('',(-88.5,207.5,144.874999999999));
#31354=CARTESIAN_POINT('Origin',(-88.5,207.5,135.874999999999));
#31355=CARTESIAN_POINT('',(-88.5,191.625,144.874999999999));
#31356=CARTESIAN_POINT('',(-88.5,207.5,144.874999999999));
#31357=CARTESIAN_POINT('Origin',(-88.5,191.625,135.874999999999));
#31358=CARTESIAN_POINT('Origin',(88.5,207.5,135.875));
#31359=CARTESIAN_POINT('',(88.5,207.5,144.875));
#31360=CARTESIAN_POINT('Origin',(88.5,207.5,135.875));
#31361=CARTESIAN_POINT('',(88.5,191.625,144.875));
#31362=CARTESIAN_POINT('',(88.5,207.5,144.875));
#31363=CARTESIAN_POINT('Origin',(88.5,191.625,135.875));
#31364=CARTESIAN_POINT('Origin',(265.5,207.5,135.875000000001));
#31365=CARTESIAN_POINT('',(265.5,207.5,144.875000000001));
#31366=CARTESIAN_POINT('Origin',(265.5,207.5,135.875000000001));
#31367=CARTESIAN_POINT('',(265.5,191.625,144.875000000001));
#31368=CARTESIAN_POINT('',(265.5,207.5,144.875000000001));
#31369=CARTESIAN_POINT('Origin',(265.5,191.625,135.875000000001));
#31370=CARTESIAN_POINT('Origin',(-579.2,207.5,65.8749999999998));
#31371=CARTESIAN_POINT('',(-579.2,207.5,74.8749999999998));
#31372=CARTESIAN_POINT('Origin',(-579.2,207.5,65.8749999999998));
#31373=CARTESIAN_POINT('',(-579.2,191.625,74.8749999999998));
#31374=CARTESIAN_POINT('',(-579.2,207.5,74.8749999999998));
#31375=CARTESIAN_POINT('Origin',(-579.2,191.625,65.8749999999998));
#31376=CARTESIAN_POINT('Origin',(579.2,207.5,65.8749999999999));
#31377=CARTESIAN_POINT('',(579.2,207.5,74.8749999999999));
#31378=CARTESIAN_POINT('Origin',(579.2,207.5,65.8749999999999));
#31379=CARTESIAN_POINT('',(579.2,191.625,74.8749999999999));
#31380=CARTESIAN_POINT('',(579.2,207.5,74.8749999999999));
#31381=CARTESIAN_POINT('Origin',(579.2,191.625,65.8749999999999));
#31382=CARTESIAN_POINT('Origin',(595.7,207.5,15.8749999999999));
#31383=CARTESIAN_POINT('',(595.7,191.625,15.8749999999999));
#31384=CARTESIAN_POINT('',(595.7,191.625,152.875));
#31385=CARTESIAN_POINT('',(595.7,191.625,15.8749999999999));
#31386=CARTESIAN_POINT('',(595.7,207.5,15.8749999999999));
#31387=CARTESIAN_POINT('',(595.7,207.5,15.8749999999999));
#31388=CARTESIAN_POINT('',(595.7,207.5,152.875));
#31389=CARTESIAN_POINT('',(595.7,207.5,15.8749999999999));
#31390=CARTESIAN_POINT('',(595.7,207.5,152.875));
#31391=CARTESIAN_POINT('Origin',(595.7,207.5,15.8749999999999));
#31392=CARTESIAN_POINT('',(-595.7,191.625,15.8749999999997));
#31393=CARTESIAN_POINT('',(595.7,191.625,15.8749999999999));
#31394=CARTESIAN_POINT('',(-595.7,207.5,15.8749999999997));
#31395=CARTESIAN_POINT('',(-595.7,207.5,15.8749999999997));
#31396=CARTESIAN_POINT('',(595.7,207.5,15.8749999999999));
#31397=CARTESIAN_POINT('Origin',(-595.7,207.5,15.8749999999997));
#31398=CARTESIAN_POINT('',(-595.7,191.625,152.875));
#31399=CARTESIAN_POINT('',(-595.7,191.625,15.8749999999997));
#31400=CARTESIAN_POINT('',(-595.7,207.5,152.875));
#31401=CARTESIAN_POINT('',(-595.7,207.5,152.875));
#31402=CARTESIAN_POINT('',(-595.7,207.5,15.8749999999997));
#31403=CARTESIAN_POINT('Origin',(595.7,207.5,152.875));
#31404=CARTESIAN_POINT('',(595.7,191.625,152.875));
#31405=CARTESIAN_POINT('',(595.7,207.5,152.875));
#31406=CARTESIAN_POINT('Origin',(0.,207.5,0.));
#31407=CARTESIAN_POINT('Origin',(0.,191.625,0.));
#31408=CARTESIAN_POINT('Origin',(463.699999999996,277.5,-360.509999999995));
#31409=CARTESIAN_POINT('',(463.699999999996,277.5,-347.809999999995));
#31410=CARTESIAN_POINT('',(566.699999999996,232.5,-347.809999999995));
#31411=CARTESIAN_POINT('',(463.699999999996,277.5,-347.809999999995));
#31412=CARTESIAN_POINT('',(566.699999999996,232.5,-360.509999999995));
#31413=CARTESIAN_POINT('',(566.699999999996,232.5,-360.509999999995));
#31414=CARTESIAN_POINT('',(463.699999999996,277.5,-360.509999999995));
#31415=CARTESIAN_POINT('',(463.699999999996,277.5,-360.509999999995));
#31416=CARTESIAN_POINT('',(463.699999999996,277.5,-360.509999999995));
#31417=CARTESIAN_POINT('Origin',(566.699999999996,232.5,-360.509999999995));
#31418=CARTESIAN_POINT('',(566.699999999996,207.5,-347.809999999995));
#31419=CARTESIAN_POINT('',(566.699999999996,232.5,-347.809999999995));
#31420=CARTESIAN_POINT('',(566.699999999996,207.5,-360.509999999995));
#31421=CARTESIAN_POINT('',(566.699999999996,207.5,-360.509999999995));
#31422=CARTESIAN_POINT('',(566.699999999996,232.5,-360.509999999995));
#31423=CARTESIAN_POINT('Origin',(566.699999999996,207.5,-360.509999999995));
#31424=CARTESIAN_POINT('',(422.699999999996,207.5,-347.809999999995));
#31425=CARTESIAN_POINT('',(566.699999999996,207.5,-347.809999999995));
#31426=CARTESIAN_POINT('',(422.699999999996,207.5,-360.509999999995));
#31427=CARTESIAN_POINT('',(422.699999999996,207.5,-360.509999999995));
#31428=CARTESIAN_POINT('',(566.699999999996,207.5,-360.509999999995));
#31429=CARTESIAN_POINT('Origin',(422.699999999996,207.5,-360.509999999995));
#31430=CARTESIAN_POINT('',(412.699999999996,217.5,-347.809999999995));
#31431=CARTESIAN_POINT('',(422.699999999996,207.5,-347.809999999995));
#31432=CARTESIAN_POINT('',(412.699999999996,217.5,-360.509999999995));
#31433=CARTESIAN_POINT('',(412.699999999996,217.5,-360.509999999995));
#31434=CARTESIAN_POINT('',(422.699999999996,207.5,-360.509999999995));
#31435=CARTESIAN_POINT('Origin',(412.699999999996,217.5,-360.509999999995));
#31436=CARTESIAN_POINT('',(412.699999999996,267.5,-347.809999999995));
#31437=CARTESIAN_POINT('',(412.699999999996,217.5,-347.809999999995));
#31438=CARTESIAN_POINT('',(412.699999999996,267.5,-360.509999999995));
#31439=CARTESIAN_POINT('',(412.699999999996,267.5,-360.509999999995));
#31440=CARTESIAN_POINT('',(412.699999999996,217.5,-360.509999999995));
#31441=CARTESIAN_POINT('Origin',(412.699999999996,267.5,-360.509999999995));
#31442=CARTESIAN_POINT('',(422.699999999996,277.5,-347.809999999995));
#31443=CARTESIAN_POINT('',(412.699999999996,267.5,-347.809999999995));
#31444=CARTESIAN_POINT('',(422.699999999996,277.5,-360.509999999995));
#31445=CARTESIAN_POINT('',(422.699999999996,277.5,-360.509999999995));
#31446=CARTESIAN_POINT('',(412.699999999996,267.5,-360.509999999995));
#31447=CARTESIAN_POINT('Origin',(422.699999999996,277.5,-360.509999999995));
#31448=CARTESIAN_POINT('',(422.699999999996,277.5,-347.809999999995));
#31449=CARTESIAN_POINT('',(422.699999999996,277.5,-360.509999999995));
#31450=CARTESIAN_POINT('Origin',(0.,0.,-360.509999999995));
#31451=CARTESIAN_POINT('Origin',(0.,0.,-347.809999999995));
#31452=CARTESIAN_POINT('Origin',(463.699999999997,277.5,-240.509999999995));
#31453=CARTESIAN_POINT('',(463.699999999997,277.5,-227.809999999995));
#31454=CARTESIAN_POINT('',(566.699999999997,232.5,-227.809999999995));
#31455=CARTESIAN_POINT('',(463.699999999997,277.5,-227.809999999995));
#31456=CARTESIAN_POINT('',(566.699999999997,232.5,-240.509999999995));
#31457=CARTESIAN_POINT('',(566.699999999997,232.5,-240.509999999995));
#31458=CARTESIAN_POINT('',(463.699999999997,277.5,-240.509999999995));
#31459=CARTESIAN_POINT('',(463.699999999997,277.5,-240.509999999995));
#31460=CARTESIAN_POINT('',(463.699999999997,277.5,-240.509999999995));
#31461=CARTESIAN_POINT('Origin',(566.699999999997,232.5,-240.509999999995));
#31462=CARTESIAN_POINT('',(566.699999999997,207.5,-227.809999999995));
#31463=CARTESIAN_POINT('',(566.699999999997,232.5,-227.809999999995));
#31464=CARTESIAN_POINT('',(566.699999999997,207.5,-240.509999999995));
#31465=CARTESIAN_POINT('',(566.699999999997,207.5,-240.509999999995));
#31466=CARTESIAN_POINT('',(566.699999999997,232.5,-240.509999999995));
#31467=CARTESIAN_POINT('Origin',(566.699999999997,207.5,-240.509999999995));
#31468=CARTESIAN_POINT('',(422.699999999998,207.5,-227.809999999995));
#31469=CARTESIAN_POINT('',(566.699999999997,207.5,-227.809999999995));
#31470=CARTESIAN_POINT('',(422.699999999998,207.5,-240.509999999995));
#31471=CARTESIAN_POINT('',(422.699999999998,207.5,-240.509999999995));
#31472=CARTESIAN_POINT('',(566.699999999997,207.5,-240.509999999995));
#31473=CARTESIAN_POINT('Origin',(422.699999999998,207.5,-240.509999999995));
#31474=CARTESIAN_POINT('',(412.699999999998,217.5,-227.809999999995));
#31475=CARTESIAN_POINT('',(422.699999999998,207.5,-227.809999999995));
#31476=CARTESIAN_POINT('',(412.699999999998,217.5,-240.509999999995));
#31477=CARTESIAN_POINT('',(412.699999999998,217.5,-240.509999999995));
#31478=CARTESIAN_POINT('',(422.699999999998,207.5,-240.509999999995));
#31479=CARTESIAN_POINT('Origin',(412.699999999998,217.5,-240.509999999995));
#31480=CARTESIAN_POINT('',(412.699999999998,267.5,-227.809999999995));
#31481=CARTESIAN_POINT('',(412.699999999998,217.5,-227.809999999995));
#31482=CARTESIAN_POINT('',(412.699999999998,267.5,-240.509999999995));
#31483=CARTESIAN_POINT('',(412.699999999998,267.5,-240.509999999995));
#31484=CARTESIAN_POINT('',(412.699999999998,217.5,-240.509999999995));
#31485=CARTESIAN_POINT('Origin',(412.699999999998,267.5,-240.509999999995));
#31486=CARTESIAN_POINT('',(422.699999999998,277.5,-227.809999999995));
#31487=CARTESIAN_POINT('',(412.699999999998,267.5,-227.809999999995));
#31488=CARTESIAN_POINT('',(422.699999999998,277.5,-240.509999999995));
#31489=CARTESIAN_POINT('',(422.699999999998,277.5,-240.509999999995));
#31490=CARTESIAN_POINT('',(412.699999999998,267.5,-240.509999999995));
#31491=CARTESIAN_POINT('Origin',(422.699999999998,277.5,-240.509999999995));
#31492=CARTESIAN_POINT('',(422.699999999998,277.5,-227.809999999995));
#31493=CARTESIAN_POINT('',(422.699999999998,277.5,-240.509999999995));
#31494=CARTESIAN_POINT('Origin',(1.24988860768035E-12,0.,-240.509999999995));
#31495=CARTESIAN_POINT('Origin',(1.24988860768035E-12,0.,-227.809999999995));
#31496=CARTESIAN_POINT('Origin',(463.699999999999,277.5,-120.509999999995));
#31497=CARTESIAN_POINT('',(463.699999999999,277.5,-107.809999999995));
#31498=CARTESIAN_POINT('',(566.699999999999,232.5,-107.809999999995));
#31499=CARTESIAN_POINT('',(463.699999999999,277.5,-107.809999999995));
#31500=CARTESIAN_POINT('',(566.699999999999,232.5,-120.509999999995));
#31501=CARTESIAN_POINT('',(566.699999999999,232.5,-120.509999999995));
#31502=CARTESIAN_POINT('',(463.699999999999,277.5,-120.509999999995));
#31503=CARTESIAN_POINT('',(463.699999999999,277.5,-120.509999999995));
#31504=CARTESIAN_POINT('',(463.699999999999,277.5,-120.509999999995));
#31505=CARTESIAN_POINT('Origin',(566.699999999999,232.5,-120.509999999995));
#31506=CARTESIAN_POINT('',(566.699999999999,207.5,-107.809999999995));
#31507=CARTESIAN_POINT('',(566.699999999999,232.5,-107.809999999995));
#31508=CARTESIAN_POINT('',(566.699999999999,207.5,-120.509999999995));
#31509=CARTESIAN_POINT('',(566.699999999999,207.5,-120.509999999995));
#31510=CARTESIAN_POINT('',(566.699999999999,232.5,-120.509999999995));
#31511=CARTESIAN_POINT('Origin',(566.699999999999,207.5,-120.509999999995));
#31512=CARTESIAN_POINT('',(422.699999999999,207.5,-107.809999999995));
#31513=CARTESIAN_POINT('',(566.699999999999,207.5,-107.809999999995));
#31514=CARTESIAN_POINT('',(422.699999999999,207.5,-120.509999999995));
#31515=CARTESIAN_POINT('',(422.699999999999,207.5,-120.509999999995));
#31516=CARTESIAN_POINT('',(566.699999999999,207.5,-120.509999999995));
#31517=CARTESIAN_POINT('Origin',(422.699999999999,207.5,-120.509999999995));
#31518=CARTESIAN_POINT('',(412.699999999999,217.5,-107.809999999995));
#31519=CARTESIAN_POINT('',(422.699999999999,207.5,-107.809999999995));
#31520=CARTESIAN_POINT('',(412.699999999999,217.5,-120.509999999995));
#31521=CARTESIAN_POINT('',(412.699999999999,217.5,-120.509999999995));
#31522=CARTESIAN_POINT('',(422.699999999999,207.5,-120.509999999995));
#31523=CARTESIAN_POINT('Origin',(412.699999999999,217.5,-120.509999999995));
#31524=CARTESIAN_POINT('',(412.699999999999,267.5,-107.809999999995));
#31525=CARTESIAN_POINT('',(412.699999999999,217.5,-107.809999999995));
#31526=CARTESIAN_POINT('',(412.699999999999,267.5,-120.509999999995));
#31527=CARTESIAN_POINT('',(412.699999999999,267.5,-120.509999999995));
#31528=CARTESIAN_POINT('',(412.699999999999,217.5,-120.509999999995));
#31529=CARTESIAN_POINT('Origin',(412.699999999999,267.5,-120.509999999995));
#31530=CARTESIAN_POINT('',(422.699999999999,277.5,-107.809999999995));
#31531=CARTESIAN_POINT('',(412.699999999999,267.5,-107.809999999995));
#31532=CARTESIAN_POINT('',(422.699999999999,277.5,-120.509999999995));
#31533=CARTESIAN_POINT('',(422.699999999999,277.5,-120.509999999995));
#31534=CARTESIAN_POINT('',(412.699999999999,267.5,-120.509999999995));
#31535=CARTESIAN_POINT('Origin',(422.699999999999,277.5,-120.509999999995));
#31536=CARTESIAN_POINT('',(422.699999999999,277.5,-107.809999999995));
#31537=CARTESIAN_POINT('',(422.699999999999,277.5,-120.509999999995));
#31538=CARTESIAN_POINT('Origin',(2.49977721536069E-12,0.,-120.509999999995));
#31539=CARTESIAN_POINT('Origin',(2.49977721536069E-12,0.,-107.809999999995));
#31540=CARTESIAN_POINT('Origin',(-6.35,277.5,66.6749999999998));
#31541=CARTESIAN_POINT('',(6.35,277.5,66.6749999999998));
#31542=CARTESIAN_POINT('',(6.35,232.5,152.875));
#31543=CARTESIAN_POINT('',(6.35,277.5,66.6749999999998));
#31544=CARTESIAN_POINT('',(-6.35,277.5,66.6749999999998));
#31545=CARTESIAN_POINT('',(-6.35,277.5,66.6749999999998));
#31546=CARTESIAN_POINT('',(-6.35,232.5,152.875));
#31547=CARTESIAN_POINT('',(-6.35,277.5,66.6749999999998));
#31548=CARTESIAN_POINT('',(-6.35,232.5,152.875));
#31549=CARTESIAN_POINT('Origin',(-6.35,277.5,25.8749999999999));
#31550=CARTESIAN_POINT('',(6.35,277.5,25.8749999999999));
#31551=CARTESIAN_POINT('',(6.35,277.5,25.8749999999999));
#31552=CARTESIAN_POINT('',(-6.35,277.5,25.8749999999999));
#31553=CARTESIAN_POINT('',(-6.35,277.5,25.8749999999999));
#31554=CARTESIAN_POINT('',(-6.35,277.5,25.8749999999999));
#31555=CARTESIAN_POINT('Origin',(-6.35,267.5,15.875));
#31556=CARTESIAN_POINT('',(6.35,267.5,15.875));
#31557=CARTESIAN_POINT('',(6.35,267.5,15.875));
#31558=CARTESIAN_POINT('',(-6.35,267.5,15.875));
#31559=CARTESIAN_POINT('',(-6.35,267.5,15.875));
#31560=CARTESIAN_POINT('',(-6.35,267.5,15.875));
#31561=CARTESIAN_POINT('Origin',(-6.35,217.5,15.875));
#31562=CARTESIAN_POINT('',(6.35,217.5,15.875));
#31563=CARTESIAN_POINT('',(6.35,217.5,15.875));
#31564=CARTESIAN_POINT('',(-6.35,217.5,15.875));
#31565=CARTESIAN_POINT('',(-6.35,217.5,15.875));
#31566=CARTESIAN_POINT('',(-6.35,217.5,15.875));
#31567=CARTESIAN_POINT('Origin',(-6.35,207.5,25.875));
#31568=CARTESIAN_POINT('',(6.35,207.5,25.875));
#31569=CARTESIAN_POINT('',(6.35,207.5,25.875));
#31570=CARTESIAN_POINT('',(-6.35,207.5,25.875));
#31571=CARTESIAN_POINT('',(-6.35,207.5,25.875));
#31572=CARTESIAN_POINT('',(-6.35,207.5,25.875));
#31573=CARTESIAN_POINT('Origin',(-6.35,207.5,152.875));
#31574=CARTESIAN_POINT('',(6.35,207.5,152.875));
#31575=CARTESIAN_POINT('',(6.35,207.5,152.875));
#31576=CARTESIAN_POINT('',(-6.35,207.5,152.875));
#31577=CARTESIAN_POINT('',(-6.35,207.5,152.875));
#31578=CARTESIAN_POINT('',(-6.35,207.5,152.875));
#31579=CARTESIAN_POINT('Origin',(-6.35,232.5,152.875));
#31580=CARTESIAN_POINT('',(6.35,232.5,152.875));
#31581=CARTESIAN_POINT('',(-6.35,232.5,152.875));
#31582=CARTESIAN_POINT('Origin',(-6.35,0.,0.));
#31583=CARTESIAN_POINT('Origin',(6.35,0.,0.));
#31584=CARTESIAN_POINT('Origin',(170.65,277.5,66.6749999999998));
#31585=CARTESIAN_POINT('',(183.35,277.5,66.6749999999998));
#31586=CARTESIAN_POINT('',(183.35,232.5,152.875));
#31587=CARTESIAN_POINT('',(183.35,277.5,66.6749999999998));
#31588=CARTESIAN_POINT('',(170.65,277.5,66.6749999999998));
#31589=CARTESIAN_POINT('',(170.65,277.5,66.6749999999998));
#31590=CARTESIAN_POINT('',(170.65,232.5,152.875));
#31591=CARTESIAN_POINT('',(170.65,277.5,66.6749999999998));
#31592=CARTESIAN_POINT('',(170.65,232.5,152.875));
#31593=CARTESIAN_POINT('Origin',(170.65,277.5,25.8749999999999));
#31594=CARTESIAN_POINT('',(183.35,277.5,25.8749999999999));
#31595=CARTESIAN_POINT('',(183.35,277.5,25.8749999999999));
#31596=CARTESIAN_POINT('',(170.65,277.5,25.8749999999999));
#31597=CARTESIAN_POINT('',(170.65,277.5,25.8749999999999));
#31598=CARTESIAN_POINT('',(170.65,277.5,25.8749999999999));
#31599=CARTESIAN_POINT('Origin',(170.65,267.5,15.875));
#31600=CARTESIAN_POINT('',(183.35,267.5,15.875));
#31601=CARTESIAN_POINT('',(183.35,267.5,15.875));
#31602=CARTESIAN_POINT('',(170.65,267.5,15.875));
#31603=CARTESIAN_POINT('',(170.65,267.5,15.875));
#31604=CARTESIAN_POINT('',(170.65,267.5,15.875));
#31605=CARTESIAN_POINT('Origin',(170.65,217.5,15.875));
#31606=CARTESIAN_POINT('',(183.35,217.5,15.875));
#31607=CARTESIAN_POINT('',(183.35,217.5,15.875));
#31608=CARTESIAN_POINT('',(170.65,217.5,15.875));
#31609=CARTESIAN_POINT('',(170.65,217.5,15.875));
#31610=CARTESIAN_POINT('',(170.65,217.5,15.875));
#31611=CARTESIAN_POINT('Origin',(170.65,207.5,25.875));
#31612=CARTESIAN_POINT('',(183.35,207.5,25.875));
#31613=CARTESIAN_POINT('',(183.35,207.5,25.875));
#31614=CARTESIAN_POINT('',(170.65,207.5,25.875));
#31615=CARTESIAN_POINT('',(170.65,207.5,25.875));
#31616=CARTESIAN_POINT('',(170.65,207.5,25.875));
#31617=CARTESIAN_POINT('Origin',(170.65,207.5,152.875));
#31618=CARTESIAN_POINT('',(183.35,207.5,152.875));
#31619=CARTESIAN_POINT('',(183.35,207.5,152.875));
#31620=CARTESIAN_POINT('',(170.65,207.5,152.875));
#31621=CARTESIAN_POINT('',(170.65,207.5,152.875));
#31622=CARTESIAN_POINT('',(170.65,207.5,152.875));
#31623=CARTESIAN_POINT('Origin',(170.65,232.5,152.875));
#31624=CARTESIAN_POINT('',(183.35,232.5,152.875));
#31625=CARTESIAN_POINT('',(170.65,232.5,152.875));
#31626=CARTESIAN_POINT('Origin',(170.65,0.,0.));
#31627=CARTESIAN_POINT('Origin',(183.35,0.,0.));
#31628=CARTESIAN_POINT('Origin',(347.65,277.5,66.6749999999998));
#31629=CARTESIAN_POINT('',(360.35,277.5,66.6749999999998));
#31630=CARTESIAN_POINT('',(360.35,232.5,152.875));
#31631=CARTESIAN_POINT('',(360.35,277.5,66.6749999999998));
#31632=CARTESIAN_POINT('',(347.65,277.5,66.6749999999998));
#31633=CARTESIAN_POINT('',(347.65,277.5,66.6749999999998));
#31634=CARTESIAN_POINT('',(347.65,232.5,152.875));
#31635=CARTESIAN_POINT('',(347.65,277.5,66.6749999999998));
#31636=CARTESIAN_POINT('',(347.65,232.5,152.875));
#31637=CARTESIAN_POINT('Origin',(347.65,277.5,25.8749999999999));
#31638=CARTESIAN_POINT('',(360.35,277.5,25.8749999999999));
#31639=CARTESIAN_POINT('',(360.35,277.5,25.8749999999999));
#31640=CARTESIAN_POINT('',(347.65,277.5,25.8749999999999));
#31641=CARTESIAN_POINT('',(347.65,277.5,25.8749999999999));
#31642=CARTESIAN_POINT('',(347.65,277.5,25.8749999999999));
#31643=CARTESIAN_POINT('Origin',(347.65,267.5,15.875));
#31644=CARTESIAN_POINT('',(360.35,267.5,15.875));
#31645=CARTESIAN_POINT('',(360.35,267.5,15.875));
#31646=CARTESIAN_POINT('',(347.65,267.5,15.875));
#31647=CARTESIAN_POINT('',(347.65,267.5,15.875));
#31648=CARTESIAN_POINT('',(347.65,267.5,15.875));
#31649=CARTESIAN_POINT('Origin',(347.65,217.5,15.875));
#31650=CARTESIAN_POINT('',(360.35,217.5,15.875));
#31651=CARTESIAN_POINT('',(360.35,217.5,15.875));
#31652=CARTESIAN_POINT('',(347.65,217.5,15.875));
#31653=CARTESIAN_POINT('',(347.65,217.5,15.875));
#31654=CARTESIAN_POINT('',(347.65,217.5,15.875));
#31655=CARTESIAN_POINT('Origin',(347.65,207.5,25.875));
#31656=CARTESIAN_POINT('',(360.35,207.5,25.875));
#31657=CARTESIAN_POINT('',(360.35,207.5,25.875));
#31658=CARTESIAN_POINT('',(347.65,207.5,25.875));
#31659=CARTESIAN_POINT('',(347.65,207.5,25.875));
#31660=CARTESIAN_POINT('',(347.65,207.5,25.875));
#31661=CARTESIAN_POINT('Origin',(347.65,207.5,152.875));
#31662=CARTESIAN_POINT('',(360.35,207.5,152.875));
#31663=CARTESIAN_POINT('',(360.35,207.5,152.875));
#31664=CARTESIAN_POINT('',(347.65,207.5,152.875));
#31665=CARTESIAN_POINT('',(347.65,207.5,152.875));
#31666=CARTESIAN_POINT('',(347.65,207.5,152.875));
#31667=CARTESIAN_POINT('Origin',(347.65,232.5,152.875));
#31668=CARTESIAN_POINT('',(360.35,232.5,152.875));
#31669=CARTESIAN_POINT('',(347.65,232.5,152.875));
#31670=CARTESIAN_POINT('Origin',(347.65,0.,0.));
#31671=CARTESIAN_POINT('Origin',(360.35,0.,0.));
#31672=CARTESIAN_POINT('Origin',(-170.65,277.5,66.6749999999998));
#31673=CARTESIAN_POINT('',(-183.35,277.5,66.6749999999998));
#31674=CARTESIAN_POINT('',(-183.35,232.5,152.875));
#31675=CARTESIAN_POINT('',(-183.35,277.5,66.6749999999998));
#31676=CARTESIAN_POINT('',(-170.65,232.5,152.875));
#31677=CARTESIAN_POINT('',(-170.65,232.5,152.875));
#31678=CARTESIAN_POINT('',(-170.65,277.5,66.6749999999998));
#31679=CARTESIAN_POINT('',(-170.65,277.5,66.6749999999998));
#31680=CARTESIAN_POINT('',(-170.65,277.5,66.6749999999998));
#31681=CARTESIAN_POINT('Origin',(-170.65,277.5,25.8749999999999));
#31682=CARTESIAN_POINT('',(-183.35,277.5,25.8749999999999));
#31683=CARTESIAN_POINT('',(-183.35,277.5,25.8749999999999));
#31684=CARTESIAN_POINT('',(-170.65,277.5,25.8749999999999));
#31685=CARTESIAN_POINT('',(-170.65,277.5,25.8749999999999));
#31686=CARTESIAN_POINT('',(-170.65,277.5,25.8749999999999));
#31687=CARTESIAN_POINT('Origin',(-170.65,267.5,15.875));
#31688=CARTESIAN_POINT('',(-183.35,267.5,15.875));
#31689=CARTESIAN_POINT('',(-183.35,267.5,15.875));
#31690=CARTESIAN_POINT('',(-170.65,267.5,15.875));
#31691=CARTESIAN_POINT('',(-170.65,267.5,15.875));
#31692=CARTESIAN_POINT('',(-170.65,267.5,15.875));
#31693=CARTESIAN_POINT('Origin',(-170.65,217.5,15.875));
#31694=CARTESIAN_POINT('',(-183.35,217.5,15.875));
#31695=CARTESIAN_POINT('',(-183.35,217.5,15.875));
#31696=CARTESIAN_POINT('',(-170.65,217.5,15.875));
#31697=CARTESIAN_POINT('',(-170.65,217.5,15.875));
#31698=CARTESIAN_POINT('',(-170.65,217.5,15.875));
#31699=CARTESIAN_POINT('Origin',(-170.65,207.5,25.875));
#31700=CARTESIAN_POINT('',(-183.35,207.5,25.875));
#31701=CARTESIAN_POINT('',(-183.35,207.5,25.875));
#31702=CARTESIAN_POINT('',(-170.65,207.5,25.875));
#31703=CARTESIAN_POINT('',(-170.65,207.5,25.875));
#31704=CARTESIAN_POINT('',(-170.65,207.5,25.875));
#31705=CARTESIAN_POINT('Origin',(-170.65,207.5,152.875));
#31706=CARTESIAN_POINT('',(-183.35,207.5,152.875));
#31707=CARTESIAN_POINT('',(-183.35,207.5,152.875));
#31708=CARTESIAN_POINT('',(-170.65,207.5,152.875));
#31709=CARTESIAN_POINT('',(-170.65,207.5,152.875));
#31710=CARTESIAN_POINT('',(-170.65,207.5,152.875));
#31711=CARTESIAN_POINT('Origin',(-170.65,232.5,152.875));
#31712=CARTESIAN_POINT('',(-183.35,232.5,152.875));
#31713=CARTESIAN_POINT('',(-170.65,232.5,152.875));
#31714=CARTESIAN_POINT('Origin',(-170.65,0.,0.));
#31715=CARTESIAN_POINT('Origin',(-183.35,0.,0.));
#31716=CARTESIAN_POINT('Origin',(-347.65,277.5,66.6749999999998));
#31717=CARTESIAN_POINT('',(-360.35,277.5,66.6749999999998));
#31718=CARTESIAN_POINT('',(-360.35,232.5,152.875));
#31719=CARTESIAN_POINT('',(-360.35,277.5,66.6749999999998));
#31720=CARTESIAN_POINT('',(-347.65,232.5,152.875));
#31721=CARTESIAN_POINT('',(-347.65,232.5,152.875));
#31722=CARTESIAN_POINT('',(-347.65,277.5,66.6749999999998));
#31723=CARTESIAN_POINT('',(-347.65,277.5,66.6749999999998));
#31724=CARTESIAN_POINT('',(-347.65,277.5,66.6749999999998));
#31725=CARTESIAN_POINT('Origin',(-347.65,277.5,25.8749999999999));
#31726=CARTESIAN_POINT('',(-360.35,277.5,25.8749999999999));
#31727=CARTESIAN_POINT('',(-360.35,277.5,25.8749999999999));
#31728=CARTESIAN_POINT('',(-347.65,277.5,25.8749999999999));
#31729=CARTESIAN_POINT('',(-347.65,277.5,25.8749999999999));
#31730=CARTESIAN_POINT('',(-347.65,277.5,25.8749999999999));
#31731=CARTESIAN_POINT('Origin',(-347.65,267.5,15.875));
#31732=CARTESIAN_POINT('',(-360.35,267.5,15.875));
#31733=CARTESIAN_POINT('',(-360.35,267.5,15.875));
#31734=CARTESIAN_POINT('',(-347.65,267.5,15.875));
#31735=CARTESIAN_POINT('',(-347.65,267.5,15.875));
#31736=CARTESIAN_POINT('',(-347.65,267.5,15.875));
#31737=CARTESIAN_POINT('Origin',(-347.65,217.5,15.875));
#31738=CARTESIAN_POINT('',(-360.35,217.5,15.875));
#31739=CARTESIAN_POINT('',(-360.35,217.5,15.875));
#31740=CARTESIAN_POINT('',(-347.65,217.5,15.875));
#31741=CARTESIAN_POINT('',(-347.65,217.5,15.875));
#31742=CARTESIAN_POINT('',(-347.65,217.5,15.875));
#31743=CARTESIAN_POINT('Origin',(-347.65,207.5,25.875));
#31744=CARTESIAN_POINT('',(-360.35,207.5,25.875));
#31745=CARTESIAN_POINT('',(-360.35,207.5,25.875));
#31746=CARTESIAN_POINT('',(-347.65,207.5,25.875));
#31747=CARTESIAN_POINT('',(-347.65,207.5,25.875));
#31748=CARTESIAN_POINT('',(-347.65,207.5,25.875));
#31749=CARTESIAN_POINT('Origin',(-347.65,207.5,152.875));
#31750=CARTESIAN_POINT('',(-360.35,207.5,152.875));
#31751=CARTESIAN_POINT('',(-360.35,207.5,152.875));
#31752=CARTESIAN_POINT('',(-347.65,207.5,152.875));
#31753=CARTESIAN_POINT('',(-347.65,207.5,152.875));
#31754=CARTESIAN_POINT('',(-347.65,207.5,152.875));
#31755=CARTESIAN_POINT('Origin',(-347.65,232.5,152.875));
#31756=CARTESIAN_POINT('',(-360.35,232.5,152.875));
#31757=CARTESIAN_POINT('',(-347.65,232.5,152.875));
#31758=CARTESIAN_POINT('Origin',(-347.65,0.,0.));
#31759=CARTESIAN_POINT('Origin',(-360.35,0.,0.));
#31760=CARTESIAN_POINT('Origin',(-463.699999999999,277.5,-120.509999999995));
#31761=CARTESIAN_POINT('',(-463.699999999999,277.5,-107.809999999995));
#31762=CARTESIAN_POINT('',(-566.699999999999,232.5,-107.809999999995));
#31763=CARTESIAN_POINT('',(-463.699999999999,277.5,-107.809999999995));
#31764=CARTESIAN_POINT('',(-463.699999999999,277.5,-120.509999999995));
#31765=CARTESIAN_POINT('',(-463.699999999999,277.5,-120.509999999995));
#31766=CARTESIAN_POINT('',(-566.699999999999,232.5,-120.509999999995));
#31767=CARTESIAN_POINT('',(-463.699999999999,277.5,-120.509999999995));
#31768=CARTESIAN_POINT('',(-566.699999999999,232.5,-120.509999999995));
#31769=CARTESIAN_POINT('Origin',(-566.699999999999,232.5,-120.509999999995));
#31770=CARTESIAN_POINT('',(-566.699999999999,207.5,-107.809999999995));
#31771=CARTESIAN_POINT('',(-566.699999999999,232.5,-107.809999999995));
#31772=CARTESIAN_POINT('',(-566.699999999999,207.5,-120.509999999995));
#31773=CARTESIAN_POINT('',(-566.699999999999,232.5,-120.509999999995));
#31774=CARTESIAN_POINT('',(-566.699999999999,207.5,-120.509999999995));
#31775=CARTESIAN_POINT('Origin',(-566.699999999999,207.5,-120.509999999995));
#31776=CARTESIAN_POINT('',(-422.699999999999,207.5,-107.809999999995));
#31777=CARTESIAN_POINT('',(-566.699999999999,207.5,-107.809999999995));
#31778=CARTESIAN_POINT('',(-422.699999999999,207.5,-120.509999999995));
#31779=CARTESIAN_POINT('',(-566.699999999999,207.5,-120.509999999995));
#31780=CARTESIAN_POINT('',(-422.699999999999,207.5,-120.509999999995));
#31781=CARTESIAN_POINT('Origin',(-422.699999999999,207.5,-120.509999999995));
#31782=CARTESIAN_POINT('',(-412.699999999999,217.5,-107.809999999995));
#31783=CARTESIAN_POINT('',(-422.699999999999,207.5,-107.809999999995));
#31784=CARTESIAN_POINT('',(-412.699999999999,217.5,-120.509999999995));
#31785=CARTESIAN_POINT('',(-422.699999999999,207.5,-120.509999999995));
#31786=CARTESIAN_POINT('',(-412.699999999999,217.5,-120.509999999995));
#31787=CARTESIAN_POINT('Origin',(-412.699999999999,217.5,-120.509999999995));
#31788=CARTESIAN_POINT('',(-412.699999999999,267.5,-107.809999999995));
#31789=CARTESIAN_POINT('',(-412.699999999999,217.5,-107.809999999995));
#31790=CARTESIAN_POINT('',(-412.699999999999,267.5,-120.509999999995));
#31791=CARTESIAN_POINT('',(-412.699999999999,217.5,-120.509999999995));
#31792=CARTESIAN_POINT('',(-412.699999999999,267.5,-120.509999999995));
#31793=CARTESIAN_POINT('Origin',(-412.699999999999,267.5,-120.509999999995));
#31794=CARTESIAN_POINT('',(-422.699999999999,277.5,-107.809999999995));
#31795=CARTESIAN_POINT('',(-412.699999999999,267.5,-107.809999999995));
#31796=CARTESIAN_POINT('',(-422.699999999999,277.5,-120.509999999995));
#31797=CARTESIAN_POINT('',(-412.699999999999,267.5,-120.509999999995));
#31798=CARTESIAN_POINT('',(-422.699999999999,277.5,-120.509999999995));
#31799=CARTESIAN_POINT('Origin',(-422.699999999999,277.5,-120.509999999995));
#31800=CARTESIAN_POINT('',(-422.699999999999,277.5,-107.809999999995));
#31801=CARTESIAN_POINT('',(-422.699999999999,277.5,-120.509999999995));
#31802=CARTESIAN_POINT('Origin',(-2.49977721536069E-12,0.,-120.509999999995));
#31803=CARTESIAN_POINT('Origin',(-2.49977721536069E-12,0.,-107.809999999995));
#31804=CARTESIAN_POINT('Origin',(-463.699999999997,277.5,-240.509999999995));
#31805=CARTESIAN_POINT('',(-463.699999999997,277.5,-227.809999999995));
#31806=CARTESIAN_POINT('',(-566.699999999997,232.5,-227.809999999995));
#31807=CARTESIAN_POINT('',(-463.699999999997,277.5,-227.809999999995));
#31808=CARTESIAN_POINT('',(-463.699999999997,277.5,-240.509999999995));
#31809=CARTESIAN_POINT('',(-463.699999999997,277.5,-240.509999999995));
#31810=CARTESIAN_POINT('',(-566.699999999997,232.5,-240.509999999995));
#31811=CARTESIAN_POINT('',(-463.699999999997,277.5,-240.509999999995));
#31812=CARTESIAN_POINT('',(-566.699999999997,232.5,-240.509999999995));
#31813=CARTESIAN_POINT('Origin',(-566.699999999997,232.5,-240.509999999995));
#31814=CARTESIAN_POINT('',(-566.699999999997,207.5,-227.809999999995));
#31815=CARTESIAN_POINT('',(-566.699999999997,232.5,-227.809999999995));
#31816=CARTESIAN_POINT('',(-566.699999999997,207.5,-240.509999999995));
#31817=CARTESIAN_POINT('',(-566.699999999997,232.5,-240.509999999995));
#31818=CARTESIAN_POINT('',(-566.699999999997,207.5,-240.509999999995));
#31819=CARTESIAN_POINT('Origin',(-566.699999999997,207.5,-240.509999999995));
#31820=CARTESIAN_POINT('',(-422.699999999998,207.5,-227.809999999995));
#31821=CARTESIAN_POINT('',(-566.699999999997,207.5,-227.809999999995));
#31822=CARTESIAN_POINT('',(-422.699999999998,207.5,-240.509999999995));
#31823=CARTESIAN_POINT('',(-566.699999999997,207.5,-240.509999999995));
#31824=CARTESIAN_POINT('',(-422.699999999998,207.5,-240.509999999995));
#31825=CARTESIAN_POINT('Origin',(-422.699999999998,207.5,-240.509999999995));
#31826=CARTESIAN_POINT('',(-412.699999999998,217.5,-227.809999999995));
#31827=CARTESIAN_POINT('',(-422.699999999998,207.5,-227.809999999995));
#31828=CARTESIAN_POINT('',(-412.699999999998,217.5,-240.509999999995));
#31829=CARTESIAN_POINT('',(-422.699999999998,207.5,-240.509999999995));
#31830=CARTESIAN_POINT('',(-412.699999999998,217.5,-240.509999999995));
#31831=CARTESIAN_POINT('Origin',(-412.699999999998,217.5,-240.509999999995));
#31832=CARTESIAN_POINT('',(-412.699999999998,267.5,-227.809999999995));
#31833=CARTESIAN_POINT('',(-412.699999999998,217.5,-227.809999999995));
#31834=CARTESIAN_POINT('',(-412.699999999998,267.5,-240.509999999995));
#31835=CARTESIAN_POINT('',(-412.699999999998,217.5,-240.509999999995));
#31836=CARTESIAN_POINT('',(-412.699999999998,267.5,-240.509999999995));
#31837=CARTESIAN_POINT('Origin',(-412.699999999998,267.5,-240.509999999995));
#31838=CARTESIAN_POINT('',(-422.699999999998,277.5,-227.809999999995));
#31839=CARTESIAN_POINT('',(-412.699999999998,267.5,-227.809999999995));
#31840=CARTESIAN_POINT('',(-422.699999999998,277.5,-240.509999999995));
#31841=CARTESIAN_POINT('',(-412.699999999998,267.5,-240.509999999995));
#31842=CARTESIAN_POINT('',(-422.699999999998,277.5,-240.509999999995));
#31843=CARTESIAN_POINT('Origin',(-422.699999999998,277.5,-240.509999999995));
#31844=CARTESIAN_POINT('',(-422.699999999998,277.5,-227.809999999995));
#31845=CARTESIAN_POINT('',(-422.699999999998,277.5,-240.509999999995));
#31846=CARTESIAN_POINT('Origin',(-1.24988860768035E-12,0.,-240.509999999995));
#31847=CARTESIAN_POINT('Origin',(-1.24988860768035E-12,0.,-227.809999999995));
#31848=CARTESIAN_POINT('Origin',(-463.699999999996,277.5,-360.509999999995));
#31849=CARTESIAN_POINT('',(-463.699999999996,277.5,-347.809999999995));
#31850=CARTESIAN_POINT('',(-566.699999999996,232.5,-347.809999999995));
#31851=CARTESIAN_POINT('',(-463.699999999996,277.5,-347.809999999995));
#31852=CARTESIAN_POINT('',(-463.699999999996,277.5,-360.509999999995));
#31853=CARTESIAN_POINT('',(-463.699999999996,277.5,-360.509999999995));
#31854=CARTESIAN_POINT('',(-566.699999999996,232.5,-360.509999999995));
#31855=CARTESIAN_POINT('',(-463.699999999996,277.5,-360.509999999995));
#31856=CARTESIAN_POINT('',(-566.699999999996,232.5,-360.509999999995));
#31857=CARTESIAN_POINT('Origin',(-566.699999999996,232.5,-360.509999999995));
#31858=CARTESIAN_POINT('',(-566.699999999996,207.5,-347.809999999995));
#31859=CARTESIAN_POINT('',(-566.699999999996,232.5,-347.809999999995));
#31860=CARTESIAN_POINT('',(-566.699999999996,207.5,-360.509999999995));
#31861=CARTESIAN_POINT('',(-566.699999999996,232.5,-360.509999999995));
#31862=CARTESIAN_POINT('',(-566.699999999996,207.5,-360.509999999995));
#31863=CARTESIAN_POINT('Origin',(-566.699999999996,207.5,-360.509999999995));
#31864=CARTESIAN_POINT('',(-422.699999999996,207.5,-347.809999999995));
#31865=CARTESIAN_POINT('',(-566.699999999996,207.5,-347.809999999995));
#31866=CARTESIAN_POINT('',(-422.699999999996,207.5,-360.509999999995));
#31867=CARTESIAN_POINT('',(-566.699999999996,207.5,-360.509999999995));
#31868=CARTESIAN_POINT('',(-422.699999999996,207.5,-360.509999999995));
#31869=CARTESIAN_POINT('Origin',(-422.699999999996,207.5,-360.509999999995));
#31870=CARTESIAN_POINT('',(-412.699999999996,217.5,-347.809999999995));
#31871=CARTESIAN_POINT('',(-422.699999999996,207.5,-347.809999999995));
#31872=CARTESIAN_POINT('',(-412.699999999996,217.5,-360.509999999995));
#31873=CARTESIAN_POINT('',(-422.699999999996,207.5,-360.509999999995));
#31874=CARTESIAN_POINT('',(-412.699999999996,217.5,-360.509999999995));
#31875=CARTESIAN_POINT('Origin',(-412.699999999996,217.5,-360.509999999995));
#31876=CARTESIAN_POINT('',(-412.699999999996,267.5,-347.809999999995));
#31877=CARTESIAN_POINT('',(-412.699999999996,217.5,-347.809999999995));
#31878=CARTESIAN_POINT('',(-412.699999999996,267.5,-360.509999999995));
#31879=CARTESIAN_POINT('',(-412.699999999996,217.5,-360.509999999995));
#31880=CARTESIAN_POINT('',(-412.699999999996,267.5,-360.509999999995));
#31881=CARTESIAN_POINT('Origin',(-412.699999999996,267.5,-360.509999999995));
#31882=CARTESIAN_POINT('',(-422.699999999996,277.5,-347.809999999995));
#31883=CARTESIAN_POINT('',(-412.699999999996,267.5,-347.809999999995));
#31884=CARTESIAN_POINT('',(-422.699999999996,277.5,-360.509999999995));
#31885=CARTESIAN_POINT('',(-412.699999999996,267.5,-360.509999999995));
#31886=CARTESIAN_POINT('',(-422.699999999996,277.5,-360.509999999995));
#31887=CARTESIAN_POINT('Origin',(-422.699999999996,277.5,-360.509999999995));
#31888=CARTESIAN_POINT('',(-422.699999999996,277.5,-347.809999999995));
#31889=CARTESIAN_POINT('',(-422.699999999996,277.5,-360.509999999995));
#31890=CARTESIAN_POINT('Origin',(0.,0.,-360.509999999995));
#31891=CARTESIAN_POINT('Origin',(0.,0.,-347.809999999995));
#31892=CARTESIAN_POINT('Origin',(-579.199999999996,191.625,-54.1249999999996));
#31893=CARTESIAN_POINT('',(-579.199999999996,191.625,-63.1249999999996));
#31894=CARTESIAN_POINT('Origin',(-579.199999999996,191.625,-54.1249999999996));
#31895=CARTESIAN_POINT('',(-579.199999999996,207.5,-63.1249999999996));
#31896=CARTESIAN_POINT('',(-579.199999999996,191.625,-63.1249999999996));
#31897=CARTESIAN_POINT('Origin',(-579.199999999996,207.5,-54.1249999999996));
#31898=CARTESIAN_POINT('Origin',(-579.199999999998,191.625,-174.125));
#31899=CARTESIAN_POINT('',(-579.199999999998,191.625,-183.125));
#31900=CARTESIAN_POINT('Origin',(-579.199999999998,191.625,-174.125));
#31901=CARTESIAN_POINT('',(-579.199999999998,207.5,-183.125));
#31902=CARTESIAN_POINT('',(-579.199999999998,191.625,-183.125));
#31903=CARTESIAN_POINT('Origin',(-579.199999999998,207.5,-174.125));
#31904=CARTESIAN_POINT('Origin',(-579.199999999999,191.625,-294.125));
#31905=CARTESIAN_POINT('',(-579.199999999999,191.625,-303.125));
#31906=CARTESIAN_POINT('Origin',(-579.199999999999,191.625,-294.125));
#31907=CARTESIAN_POINT('',(-579.199999999999,207.5,-303.125));
#31908=CARTESIAN_POINT('',(-579.199999999999,191.625,-303.125));
#31909=CARTESIAN_POINT('Origin',(-579.199999999999,207.5,-294.125));
#31910=CARTESIAN_POINT('Origin',(-579.2,191.625,-414.125));
#31911=CARTESIAN_POINT('',(-579.2,191.625,-423.125));
#31912=CARTESIAN_POINT('Origin',(-579.2,191.625,-414.125));
#31913=CARTESIAN_POINT('',(-579.2,207.5,-423.125));
#31914=CARTESIAN_POINT('',(-579.2,191.625,-423.125));
#31915=CARTESIAN_POINT('Origin',(-579.2,207.5,-414.125));
#31916=CARTESIAN_POINT('Origin',(0.,191.625,0.));
#31917=CARTESIAN_POINT('',(-412.7,191.625,15.8749999999999));
#31918=CARTESIAN_POINT('',(-412.7,191.625,-453.125));
#31919=CARTESIAN_POINT('',(-412.7,191.625,-453.125));
#31920=CARTESIAN_POINT('',(-595.7,191.625,15.8749999999999));
#31921=CARTESIAN_POINT('',(-412.7,191.625,15.8749999999999));
#31922=CARTESIAN_POINT('',(-595.7,191.625,-453.125));
#31923=CARTESIAN_POINT('',(-595.7,191.625,-453.125));
#31924=CARTESIAN_POINT('',(-412.7,191.625,-453.125));
#31925=CARTESIAN_POINT('Origin',(0.,207.5,0.));
#31926=CARTESIAN_POINT('',(-412.7,207.5,15.8749999999999));
#31927=CARTESIAN_POINT('',(-412.7,207.5,-453.125));
#31928=CARTESIAN_POINT('',(-412.7,207.5,-453.125));
#31929=CARTESIAN_POINT('',(-595.7,207.5,-453.125));
#31930=CARTESIAN_POINT('',(-412.7,207.5,-453.125));
#31931=CARTESIAN_POINT('',(-595.7,207.5,15.8749999999999));
#31932=CARTESIAN_POINT('',(-595.7,207.5,-453.125));
#31933=CARTESIAN_POINT('',(-412.7,207.5,15.8749999999999));
#31934=CARTESIAN_POINT('Origin',(-412.7,191.625,-453.125));
#31935=CARTESIAN_POINT('',(-412.7,191.625,15.8749999999999));
#31936=CARTESIAN_POINT('',(-412.7,191.625,-453.125));
#31937=CARTESIAN_POINT('Origin',(-412.7,191.625,-453.125));
#31938=CARTESIAN_POINT('',(-595.7,191.625,-453.125));
#31939=CARTESIAN_POINT('Origin',(-595.7,191.625,-453.125));
#31940=CARTESIAN_POINT('',(-595.7,191.625,15.8749999999999));
#31941=CARTESIAN_POINT('Origin',(-412.7,191.625,15.8749999999999));
#31942=CARTESIAN_POINT('Origin',(-374.6,-56.6030981210581,-692.742399072376));
#31943=CARTESIAN_POINT('',(-374.6,-63.1029956157432,-704.000788502422));
#31944=CARTESIAN_POINT('',(-374.6,-400.854678517142,-509.003863661867));
#31945=CARTESIAN_POINT('',(-374.6,-63.1029956157432,-704.000788502422));
#31946=CARTESIAN_POINT('',(-374.6,-394.354781022457,-497.74547423182));
#31947=CARTESIAN_POINT('',(-374.6,-394.354781022457,-497.74547423182));
#31948=CARTESIAN_POINT('',(-374.6,-56.6030981210581,-692.742399072376));
#31949=CARTESIAN_POINT('',(-374.6,-56.6030981210581,-692.742399072376));
#31950=CARTESIAN_POINT('',(-374.6,-56.6030981210581,-692.742399072376));
#31951=CARTESIAN_POINT('Origin',(-374.6,-394.354781022457,-497.74547423182));
#31952=CARTESIAN_POINT('',(-194.8,-400.854678517142,-509.003863661867));
#31953=CARTESIAN_POINT('',(-374.6,-400.854678517142,-509.003863661867));
#31954=CARTESIAN_POINT('',(-194.8,-394.354781022457,-497.74547423182));
#31955=CARTESIAN_POINT('',(-194.8,-394.354781022457,-497.74547423182));
#31956=CARTESIAN_POINT('',(-374.6,-394.354781022457,-497.74547423182));
#31957=CARTESIAN_POINT('Origin',(-194.8,-56.6030981210581,-692.742399072376));
#31958=CARTESIAN_POINT('',(-194.8,-63.1029956157432,-704.000788502422));
#31959=CARTESIAN_POINT('',(-194.8,-63.1029956157432,-704.000788502422));
#31960=CARTESIAN_POINT('',(-194.8,-56.6030981210581,-692.742399072376));
#31961=CARTESIAN_POINT('',(-194.8,-56.6030981210581,-692.742399072376));
#31962=CARTESIAN_POINT('',(-194.8,-56.6030981210581,-692.742399072376));
#31963=CARTESIAN_POINT('Origin',(-374.6,-56.6030981210581,-692.742399072376));
#31964=CARTESIAN_POINT('',(-374.6,-63.1029956157432,-704.000788502422));
#31965=CARTESIAN_POINT('',(-374.6,-56.6030981210581,-692.742399072376));
#31966=CARTESIAN_POINT('Origin',(0.,-314.113432458224,-544.071864320163));
#31967=CARTESIAN_POINT('Origin',(0.,-320.613329952909,-555.33025375021));
#31968=CARTESIAN_POINT('Origin',(5.,-403.015080584031,-492.745553082062));
#31969=CARTESIAN_POINT('',(5.,-409.514978078716,-504.003942512109));
#31970=CARTESIAN_POINT('',(4.99999999999989,-526.609655925898,-436.400720229833));
#31971=CARTESIAN_POINT('',(5.,-409.514978078716,-504.003942512109));
#31972=CARTESIAN_POINT('',(4.99999999999989,-520.109758431213,-425.142330799786));
#31973=CARTESIAN_POINT('',(4.99999999999989,-520.109758431213,-425.142330799786));
#31974=CARTESIAN_POINT('',(5.,-403.015080584031,-492.745553082062));
#31975=CARTESIAN_POINT('',(5.,-403.015080584031,-492.745553082062));
#31976=CARTESIAN_POINT('',(5.,-403.015080584031,-492.745553082062));
#31977=CARTESIAN_POINT('Origin',(4.99999999999989,-520.109758431213,-425.142330799786));
#31978=CARTESIAN_POINT('',(374.6,-526.609655925898,-436.400720229833));
#31979=CARTESIAN_POINT('',(4.99999999999989,-526.609655925898,-436.400720229833));
#31980=CARTESIAN_POINT('',(374.6,-520.109758431213,-425.142330799786));
#31981=CARTESIAN_POINT('',(374.6,-520.109758431213,-425.142330799786));
#31982=CARTESIAN_POINT('',(4.99999999999989,-520.109758431213,-425.142330799786));
#31983=CARTESIAN_POINT('Origin',(374.6,-403.015080584031,-492.745553082062));
#31984=CARTESIAN_POINT('',(374.6,-409.514978078716,-504.003942512109));
#31985=CARTESIAN_POINT('',(374.6,-409.514978078716,-504.003942512109));
#31986=CARTESIAN_POINT('',(374.6,-403.015080584031,-492.745553082062));
#31987=CARTESIAN_POINT('',(374.6,-403.015080584031,-492.745553082062));
#31988=CARTESIAN_POINT('',(374.6,-403.015080584031,-492.745553082062));
#31989=CARTESIAN_POINT('Origin',(5.,-403.015080584031,-492.745553082062));
#31990=CARTESIAN_POINT('',(5.,-409.514978078716,-504.003942512109));
#31991=CARTESIAN_POINT('',(5.,-403.015080584031,-492.745553082062));
#31992=CARTESIAN_POINT('Origin',(0.,-314.113432458223,-544.071864320163));
#31993=CARTESIAN_POINT('Origin',(0.,-320.613329952908,-555.33025375021));
#31994=CARTESIAN_POINT('Origin',(-184.8,-56.6030981210581,-692.742399072376));
#31995=CARTESIAN_POINT('',(-184.8,-63.1029956157432,-704.000788502422));
#31996=CARTESIAN_POINT('',(-184.8,-400.854678517142,-509.003863661867));
#31997=CARTESIAN_POINT('',(-184.8,-63.1029956157432,-704.000788502422));
#31998=CARTESIAN_POINT('',(-184.8,-394.354781022457,-497.74547423182));
#31999=CARTESIAN_POINT('',(-184.8,-394.354781022457,-497.74547423182));
#32000=CARTESIAN_POINT('',(-184.8,-56.6030981210581,-692.742399072376));
#32001=CARTESIAN_POINT('',(-184.8,-56.6030981210581,-692.742399072376));
#32002=CARTESIAN_POINT('',(-184.8,-56.6030981210581,-692.742399072376));
#32003=CARTESIAN_POINT('Origin',(-184.8,-394.354781022457,-497.74547423182));
#32004=CARTESIAN_POINT('',(-4.99999999999998,-400.854678517142,-509.003863661867));
#32005=CARTESIAN_POINT('',(-184.8,-400.854678517142,-509.003863661867));
#32006=CARTESIAN_POINT('',(-4.99999999999998,-394.354781022457,-497.74547423182));
#32007=CARTESIAN_POINT('',(-4.99999999999998,-394.354781022457,-497.74547423182));
#32008=CARTESIAN_POINT('',(-184.8,-394.354781022457,-497.74547423182));
#32009=CARTESIAN_POINT('Origin',(-4.99999999999998,-56.6030981210581,-692.742399072376));
#32010=CARTESIAN_POINT('',(-4.99999999999998,-63.1029956157432,-704.000788502422));
#32011=CARTESIAN_POINT('',(-4.99999999999998,-63.1029956157432,-704.000788502422));
#32012=CARTESIAN_POINT('',(-4.99999999999998,-56.6030981210581,-692.742399072376));
#32013=CARTESIAN_POINT('',(-4.99999999999998,-56.6030981210581,-692.742399072376));
#32014=CARTESIAN_POINT('',(-4.99999999999998,-56.6030981210581,-692.742399072376));
#32015=CARTESIAN_POINT('Origin',(-184.8,-56.6030981210581,-692.742399072376));
#32016=CARTESIAN_POINT('',(-184.8,-63.1029956157432,-704.000788502422));
#32017=CARTESIAN_POINT('',(-184.8,-56.6030981210581,-692.742399072376));
#32018=CARTESIAN_POINT('Origin',(0.,-314.113432458224,-544.071864320163));
#32019=CARTESIAN_POINT('Origin',(0.,-320.613329952909,-555.33025375021));
#32020=CARTESIAN_POINT('Origin',(5.,-56.6030981210581,-692.742399072376));
#32021=CARTESIAN_POINT('',(5.,-63.1029956157432,-704.000788502422));
#32022=CARTESIAN_POINT('',(5.,-400.854678517142,-509.003863661867));
#32023=CARTESIAN_POINT('',(5.,-63.1029956157432,-704.000788502422));
#32024=CARTESIAN_POINT('',(5.,-394.354781022457,-497.74547423182));
#32025=CARTESIAN_POINT('',(5.,-394.354781022457,-497.74547423182));
#32026=CARTESIAN_POINT('',(5.,-56.6030981210581,-692.742399072376));
#32027=CARTESIAN_POINT('',(5.,-56.6030981210581,-692.742399072376));
#32028=CARTESIAN_POINT('',(5.,-56.6030981210581,-692.742399072376));
#32029=CARTESIAN_POINT('Origin',(5.,-394.354781022457,-497.74547423182));
#32030=CARTESIAN_POINT('',(184.8,-400.854678517142,-509.003863661867));
#32031=CARTESIAN_POINT('',(5.,-400.854678517142,-509.003863661867));
#32032=CARTESIAN_POINT('',(184.8,-394.354781022457,-497.74547423182));
#32033=CARTESIAN_POINT('',(184.8,-394.354781022457,-497.74547423182));
#32034=CARTESIAN_POINT('',(5.,-394.354781022457,-497.74547423182));
#32035=CARTESIAN_POINT('Origin',(184.8,-56.6030981210581,-692.742399072376));
#32036=CARTESIAN_POINT('',(184.8,-63.1029956157432,-704.000788502422));
#32037=CARTESIAN_POINT('',(184.8,-63.1029956157432,-704.000788502422));
#32038=CARTESIAN_POINT('',(184.8,-56.6030981210581,-692.742399072376));
#32039=CARTESIAN_POINT('',(184.8,-56.6030981210581,-692.742399072376));
#32040=CARTESIAN_POINT('',(184.8,-56.6030981210581,-692.742399072376));
#32041=CARTESIAN_POINT('Origin',(5.,-56.6030981210581,-692.742399072376));
#32042=CARTESIAN_POINT('',(5.,-63.1029956157432,-704.000788502422));
#32043=CARTESIAN_POINT('',(5.,-56.6030981210581,-692.742399072376));
#32044=CARTESIAN_POINT('Origin',(0.,-314.113432458224,-544.071864320163));
#32045=CARTESIAN_POINT('Origin',(0.,-320.613329952909,-555.33025375021));
#32046=CARTESIAN_POINT('Origin',(194.8,-56.6030981210581,-692.742399072376));
#32047=CARTESIAN_POINT('',(194.8,-63.1029956157432,-704.000788502422));
#32048=CARTESIAN_POINT('',(194.8,-400.854678517142,-509.003863661867));
#32049=CARTESIAN_POINT('',(194.8,-63.1029956157432,-704.000788502422));
#32050=CARTESIAN_POINT('',(194.8,-394.354781022457,-497.74547423182));
#32051=CARTESIAN_POINT('',(194.8,-394.354781022457,-497.74547423182));
#32052=CARTESIAN_POINT('',(194.8,-56.6030981210581,-692.742399072376));
#32053=CARTESIAN_POINT('',(194.8,-56.6030981210581,-692.742399072376));
#32054=CARTESIAN_POINT('',(194.8,-56.6030981210581,-692.742399072376));
#32055=CARTESIAN_POINT('Origin',(194.8,-394.354781022457,-497.74547423182));
#32056=CARTESIAN_POINT('',(374.6,-400.854678517142,-509.003863661867));
#32057=CARTESIAN_POINT('',(194.8,-400.854678517142,-509.003863661867));
#32058=CARTESIAN_POINT('',(374.6,-394.354781022457,-497.74547423182));
#32059=CARTESIAN_POINT('',(374.6,-394.354781022457,-497.74547423182));
#32060=CARTESIAN_POINT('',(194.8,-394.354781022457,-497.74547423182));
#32061=CARTESIAN_POINT('Origin',(374.6,-56.6030981210581,-692.742399072376));
#32062=CARTESIAN_POINT('',(374.6,-63.1029956157432,-704.000788502422));
#32063=CARTESIAN_POINT('',(374.6,-63.1029956157432,-704.000788502422));
#32064=CARTESIAN_POINT('',(374.6,-56.6030981210581,-692.742399072376));
#32065=CARTESIAN_POINT('',(374.6,-56.6030981210581,-692.742399072376));
#32066=CARTESIAN_POINT('',(374.6,-56.6030981210581,-692.742399072376));
#32067=CARTESIAN_POINT('Origin',(194.8,-56.6030981210581,-692.742399072376));
#32068=CARTESIAN_POINT('',(194.8,-63.1029956157432,-704.000788502422));
#32069=CARTESIAN_POINT('',(194.8,-56.6030981210581,-692.742399072376));
#32070=CARTESIAN_POINT('Origin',(0.,-314.113432458224,-544.071864320163));
#32071=CARTESIAN_POINT('Origin',(0.,-320.613329952909,-555.33025375021));
#32072=CARTESIAN_POINT('Origin',(-374.6,-403.015080584031,-492.745553082062));
#32073=CARTESIAN_POINT('',(-374.6,-409.514978078716,-504.003942512109));
#32074=CARTESIAN_POINT('',(-374.6,-526.609655925898,-436.400720229833));
#32075=CARTESIAN_POINT('',(-374.6,-409.514978078716,-504.003942512109));
#32076=CARTESIAN_POINT('',(-374.6,-520.109758431213,-425.142330799786));
#32077=CARTESIAN_POINT('',(-374.6,-520.109758431213,-425.142330799786));
#32078=CARTESIAN_POINT('',(-374.6,-403.015080584031,-492.745553082062));
#32079=CARTESIAN_POINT('',(-374.6,-403.015080584031,-492.745553082062));
#32080=CARTESIAN_POINT('',(-374.6,-403.015080584031,-492.745553082062));
#32081=CARTESIAN_POINT('Origin',(-374.6,-520.109758431213,-425.142330799786));
#32082=CARTESIAN_POINT('',(-5.00000000000006,-526.609655925898,-436.400720229833));
#32083=CARTESIAN_POINT('',(-374.6,-526.609655925898,-436.400720229833));
#32084=CARTESIAN_POINT('',(-5.00000000000006,-520.109758431213,-425.142330799786));
#32085=CARTESIAN_POINT('',(-5.00000000000006,-520.109758431213,-425.142330799786));
#32086=CARTESIAN_POINT('',(-374.6,-520.109758431213,-425.142330799786));
#32087=CARTESIAN_POINT('Origin',(-4.99999999999995,-403.015080584031,-492.745553082062));
#32088=CARTESIAN_POINT('',(-4.99999999999995,-409.514978078716,-504.003942512109));
#32089=CARTESIAN_POINT('',(-4.99999999999995,-409.514978078716,-504.003942512109));
#32090=CARTESIAN_POINT('',(-4.99999999999995,-403.015080584031,-492.745553082062));
#32091=CARTESIAN_POINT('',(-4.99999999999995,-403.015080584031,-492.745553082062));
#32092=CARTESIAN_POINT('',(-4.99999999999995,-403.015080584031,-492.745553082062));
#32093=CARTESIAN_POINT('Origin',(-374.6,-403.015080584031,-492.745553082062));
#32094=CARTESIAN_POINT('',(-374.6,-409.514978078716,-504.003942512109));
#32095=CARTESIAN_POINT('',(-374.6,-403.015080584031,-492.745553082062));
#32096=CARTESIAN_POINT('Origin',(0.,-314.113432458223,-544.071864320163));
#32097=CARTESIAN_POINT('Origin',(0.,-320.613329952908,-555.33025375021));
#32098=CARTESIAN_POINT('Origin',(368.830769230769,-528.770057992788,-420.142409650028));
#32099=CARTESIAN_POINT('',(368.830769230769,-535.269955487473,-431.400799080075));
#32100=CARTESIAN_POINT('',(-368.830769230769,-535.269955487473,-431.400799080075));
#32101=CARTESIAN_POINT('',(368.830769230769,-535.269955487473,-431.400799080075));
#32102=CARTESIAN_POINT('',(-368.830769230769,-528.770057992788,-420.142409650028));
#32103=CARTESIAN_POINT('',(-368.830769230769,-528.770057992788,-420.142409650028));
#32104=CARTESIAN_POINT('',(368.830769230769,-528.770057992788,-420.142409650028));
#32105=CARTESIAN_POINT('',(368.830769230769,-528.770057992788,-420.142409650028));
#32106=CARTESIAN_POINT('',(368.830769230769,-528.770057992788,-420.142409650028));
#32107=CARTESIAN_POINT('Origin',(-368.830769230769,-528.770057992788,-420.142409650028));
#32108=CARTESIAN_POINT('',(-201.637568622845,-786.246777154128,-286.502310312096));
#32109=CARTESIAN_POINT('',(-368.830769230769,-535.269955487473,-431.400799080075));
#32110=CARTESIAN_POINT('',(-201.637568622845,-779.746879659443,-275.243920882049));
#32111=CARTESIAN_POINT('',(-201.637568622845,-779.746879659443,-275.243920882049));
#32112=CARTESIAN_POINT('',(-368.830769230769,-528.770057992788,-420.142409650028));
#32113=CARTESIAN_POINT('Origin',(-201.637568622845,-779.746879659443,-275.243920882049));
#32114=CARTESIAN_POINT('',(201.637568622845,-786.246777154128,-286.502310312096));
#32115=CARTESIAN_POINT('',(-201.637568622845,-786.246777154128,-286.502310312096));
#32116=CARTESIAN_POINT('',(201.637568622845,-779.746879659443,-275.243920882049));
#32117=CARTESIAN_POINT('',(201.637568622845,-779.746879659443,-275.243920882049));
#32118=CARTESIAN_POINT('',(-201.637568622845,-779.746879659443,-275.243920882049));
#32119=CARTESIAN_POINT('Origin',(201.637568622845,-779.746879659443,-275.243920882049));
#32120=CARTESIAN_POINT('',(201.637568622845,-786.246777154128,-286.502310312096));
#32121=CARTESIAN_POINT('',(201.637568622845,-779.746879659443,-275.243920882049));
#32122=CARTESIAN_POINT('Origin',(6.46395147870936E-15,-314.113432458224,
-544.071864320163));
#32123=CARTESIAN_POINT('Origin',(6.46395147870936E-15,-320.613329952909,
-555.33025375021));
#32124=CARTESIAN_POINT('Origin',(376.048949668551,-533.224282489496,-403.252604600343));
#32125=CARTESIAN_POINT('',(387.309362287183,-538.85035247782,-400.004459876868));
#32126=CARTESIAN_POINT('',(328.342112775413,-627.367186960784,-348.900316227531));
#32127=CARTESIAN_POINT('',(387.309362287183,-538.85035247782,-400.004459876868));
#32128=CARTESIAN_POINT('',(317.081700156781,-621.74111697246,-352.148460951006));
#32129=CARTESIAN_POINT('',(317.081700156781,-621.74111697246,-352.148460951006));
#32130=CARTESIAN_POINT('',(376.048949668551,-533.224282489496,-403.252604600343));
#32131=CARTESIAN_POINT('',(376.048949668551,-533.224282489496,-403.252604600343));
#32132=CARTESIAN_POINT('',(376.048949668551,-533.224282489496,-403.252604600343));
#32133=CARTESIAN_POINT('Origin',(317.081700156781,-621.74111697246,-352.148460951006));
#32134=CARTESIAN_POINT('',(328.342112775413,-517.568918512102,-158.720137855359));
#32135=CARTESIAN_POINT('',(328.342112775413,-627.367186960784,-348.900316227531));
#32136=CARTESIAN_POINT('',(317.081700156781,-511.942848523778,-161.968282578834));
#32137=CARTESIAN_POINT('',(317.081700156781,-511.942848523778,-161.968282578834));
#32138=CARTESIAN_POINT('',(317.081700156781,-621.74111697246,-352.148460951006));
#32139=CARTESIAN_POINT('Origin',(376.048949668551,-423.426014040814,-213.072426228171));
#32140=CARTESIAN_POINT('',(387.309362287183,-429.052084029138,-209.824281504696));
#32141=CARTESIAN_POINT('',(387.309362287183,-429.052084029138,-209.824281504696));
#32142=CARTESIAN_POINT('',(376.048949668551,-423.426014040814,-213.072426228171));
#32143=CARTESIAN_POINT('',(376.048949668551,-423.426014040814,-213.072426228171));
#32144=CARTESIAN_POINT('',(376.048949668551,-423.426014040814,-213.072426228171));
#32145=CARTESIAN_POINT('Origin',(376.048949668551,-533.224282489496,-403.252604600343));
#32146=CARTESIAN_POINT('',(387.309362287183,-538.85035247782,-400.004459876868));
#32147=CARTESIAN_POINT('',(376.048949668551,-533.224282489496,-403.252604600343));
#32148=CARTESIAN_POINT('Origin',(394.754129766534,-197.232058670006,113.869587829266));
#32149=CARTESIAN_POINT('Origin',(406.014542385166,-202.85812865833,117.117732552741));
#32150=CARTESIAN_POINT('Origin',(376.051116910575,-418.422839624243,-204.414004948869));
#32151=CARTESIAN_POINT('',(387.311529529207,-424.048909612567,-201.165860225394));
#32152=CARTESIAN_POINT('',(328.344280017437,-512.565744095532,-150.061716576057));
#32153=CARTESIAN_POINT('',(387.311529529207,-424.048909612567,-201.165860225394));
#32154=CARTESIAN_POINT('',(317.083867398805,-506.939674107208,-153.309861299531));
#32155=CARTESIAN_POINT('',(317.083867398805,-506.939674107208,-153.309861299531));
#32156=CARTESIAN_POINT('',(376.051116910575,-418.422839624243,-204.414004948869));
#32157=CARTESIAN_POINT('',(376.051116910575,-418.422839624243,-204.414004948869));
#32158=CARTESIAN_POINT('',(376.051116910575,-418.422839624243,-204.414004948869));
#32159=CARTESIAN_POINT('Origin',(317.083867398805,-506.939674107208,-153.309861299531));
#32160=CARTESIAN_POINT('',(328.344280017437,-402.76747564685,40.1184617961154));
#32161=CARTESIAN_POINT('',(328.344280017437,-512.565744095532,-150.061716576057));
#32162=CARTESIAN_POINT('',(317.083867398805,-397.141405658526,36.8703170726406));
#32163=CARTESIAN_POINT('',(317.083867398805,-397.141405658526,36.8703170726406));
#32164=CARTESIAN_POINT('',(317.083867398805,-506.939674107208,-153.309861299531));
#32165=CARTESIAN_POINT('Origin',(376.051116910575,-308.624571175561,-14.2338265766968));
#32166=CARTESIAN_POINT('',(387.311529529207,-314.250641163885,-10.985681853222));
#32167=CARTESIAN_POINT('',(387.311529529207,-314.250641163885,-10.985681853222));
#32168=CARTESIAN_POINT('',(376.051116910575,-308.624571175561,-14.2338265766968));
#32169=CARTESIAN_POINT('',(376.051116910575,-308.624571175561,-14.2338265766968));
#32170=CARTESIAN_POINT('',(376.051116910575,-308.624571175561,-14.2338265766968));
#32171=CARTESIAN_POINT('Origin',(376.051116910575,-418.422839624243,-204.414004948869));
#32172=CARTESIAN_POINT('',(387.311529529207,-424.048909612567,-201.165860225394));
#32173=CARTESIAN_POINT('',(376.051116910575,-418.422839624243,-204.414004948869));
#32174=CARTESIAN_POINT('Origin',(394.756297008558,-82.4306158047535,312.70818748074));
#32175=CARTESIAN_POINT('Origin',(406.016709627189,-88.0566857930775,315.956332204215));
#32176=CARTESIAN_POINT('Origin',(312.084475633296,-629.241334735898,-347.815507460388));
#32177=CARTESIAN_POINT('',(323.344888251928,-634.867404724222,-344.567362736913));
#32178=CARTESIAN_POINT('',(264.377638740158,-723.384239207187,-293.463219087576));
#32179=CARTESIAN_POINT('',(323.344888251928,-634.867404724222,-344.567362736913));
#32180=CARTESIAN_POINT('',(253.117226121526,-717.758169218862,-296.711363811051));
#32181=CARTESIAN_POINT('',(253.117226121526,-717.758169218862,-296.711363811051));
#32182=CARTESIAN_POINT('',(312.084475633296,-629.241334735898,-347.815507460388));
#32183=CARTESIAN_POINT('',(312.084475633296,-629.241334735898,-347.815507460388));
#32184=CARTESIAN_POINT('',(312.084475633296,-629.241334735898,-347.815507460388));
#32185=CARTESIAN_POINT('Origin',(253.117226121526,-717.758169218862,-296.711363811051));
#32186=CARTESIAN_POINT('',(264.377638740158,-613.585970758505,-103.283040715404));
#32187=CARTESIAN_POINT('',(264.377638740158,-723.384239207187,-293.463219087576));
#32188=CARTESIAN_POINT('',(253.117226121526,-607.959900770181,-106.531185438879));
#32189=CARTESIAN_POINT('',(253.117226121526,-607.959900770181,-106.531185438879));
#32190=CARTESIAN_POINT('',(253.117226121526,-717.758169218862,-296.711363811051));
#32191=CARTESIAN_POINT('Origin',(312.084475633296,-519.443066287216,-157.635329088216));
#32192=CARTESIAN_POINT('',(323.344888251928,-525.06913627554,-154.387184364741));
#32193=CARTESIAN_POINT('',(323.344888251928,-525.06913627554,-154.387184364741));
#32194=CARTESIAN_POINT('',(312.084475633296,-519.443066287216,-157.635329088216));
#32195=CARTESIAN_POINT('',(312.084475633296,-519.443066287216,-157.635329088216));
#32196=CARTESIAN_POINT('',(312.084475633296,-519.443066287216,-157.635329088216));
#32197=CARTESIAN_POINT('Origin',(312.084475633296,-629.241334735898,-347.815507460388));
#32198=CARTESIAN_POINT('',(323.344888251928,-634.867404724222,-344.567362736913));
#32199=CARTESIAN_POINT('',(312.084475633296,-629.241334735898,-347.815507460388));
#32200=CARTESIAN_POINT('Origin',(330.789655731279,-293.249110916408,169.306684969221));
#32201=CARTESIAN_POINT('Origin',(342.050068349911,-298.875180904732,172.554829692696));
#32202=CARTESIAN_POINT('Origin',(312.08664287532,-514.439891870646,-148.976907808914));
#32203=CARTESIAN_POINT('',(323.347055493952,-520.06596185897,-145.728763085439));
#32204=CARTESIAN_POINT('',(264.379805982182,-608.582796341934,-94.6246194361014));
#32205=CARTESIAN_POINT('',(323.347055493952,-520.06596185897,-145.728763085439));
#32206=CARTESIAN_POINT('',(253.11939336355,-602.95672635361,-97.8727641595762));
#32207=CARTESIAN_POINT('',(253.11939336355,-602.95672635361,-97.8727641595762));
#32208=CARTESIAN_POINT('',(312.08664287532,-514.439891870646,-148.976907808914));
#32209=CARTESIAN_POINT('',(312.08664287532,-514.439891870646,-148.976907808914));
#32210=CARTESIAN_POINT('',(312.08664287532,-514.439891870646,-148.976907808914));
#32211=CARTESIAN_POINT('Origin',(253.11939336355,-602.95672635361,-97.8727641595762));
#32212=CARTESIAN_POINT('',(264.379805982182,-498.784527893252,95.5555589360706));
#32213=CARTESIAN_POINT('',(264.379805982182,-608.582796341934,-94.6246194361014));
#32214=CARTESIAN_POINT('',(253.11939336355,-493.158457904928,92.3074142125958));
#32215=CARTESIAN_POINT('',(253.11939336355,-493.158457904928,92.3074142125958));
#32216=CARTESIAN_POINT('',(253.11939336355,-602.95672635361,-97.8727641595762));
#32217=CARTESIAN_POINT('Origin',(312.08664287532,-404.641623421964,41.2032705632584));
#32218=CARTESIAN_POINT('',(323.347055493952,-410.267693410288,44.4514152867332));
#32219=CARTESIAN_POINT('',(323.347055493952,-410.267693410288,44.4514152867332));
#32220=CARTESIAN_POINT('',(312.08664287532,-404.641623421964,41.2032705632584));
#32221=CARTESIAN_POINT('',(312.08664287532,-404.641623421964,41.2032705632584));
#32222=CARTESIAN_POINT('',(312.08664287532,-404.641623421964,41.2032705632584));
#32223=CARTESIAN_POINT('Origin',(312.08664287532,-514.439891870646,-148.976907808914));
#32224=CARTESIAN_POINT('',(323.347055493952,-520.06596185897,-145.728763085439));
#32225=CARTESIAN_POINT('',(312.08664287532,-514.439891870646,-148.976907808914));
#32226=CARTESIAN_POINT('Origin',(330.791822973303,-178.447668051156,368.145284620695));
#32227=CARTESIAN_POINT('Origin',(342.052235591935,-184.07373803948,371.39342934417));
#32228=CARTESIAN_POINT('Origin',(-376.048949668551,-533.224282489496,-403.252604600343));
#32229=CARTESIAN_POINT('',(-387.309362287183,-538.85035247782,-400.004459876868));
#32230=CARTESIAN_POINT('',(-328.342112775413,-627.367186960784,-348.900316227531));
#32231=CARTESIAN_POINT('',(-387.309362287183,-538.85035247782,-400.004459876868));
#32232=CARTESIAN_POINT('',(-376.048949668551,-533.224282489496,-403.252604600343));
#32233=CARTESIAN_POINT('',(-376.048949668551,-533.224282489496,-403.252604600343));
#32234=CARTESIAN_POINT('',(-317.081700156781,-621.74111697246,-352.148460951006));
#32235=CARTESIAN_POINT('',(-376.048949668551,-533.224282489496,-403.252604600343));
#32236=CARTESIAN_POINT('',(-317.081700156781,-621.74111697246,-352.148460951006));
#32237=CARTESIAN_POINT('Origin',(-317.081700156781,-621.74111697246,-352.148460951006));
#32238=CARTESIAN_POINT('',(-328.342112775413,-517.568918512102,-158.720137855359));
#32239=CARTESIAN_POINT('',(-328.342112775413,-627.367186960784,-348.900316227531));
#32240=CARTESIAN_POINT('',(-317.081700156781,-511.942848523778,-161.968282578834));
#32241=CARTESIAN_POINT('',(-317.081700156781,-621.74111697246,-352.148460951006));
#32242=CARTESIAN_POINT('',(-317.081700156781,-511.942848523778,-161.968282578834));
#32243=CARTESIAN_POINT('Origin',(-376.048949668551,-423.426014040814,-213.072426228171));
#32244=CARTESIAN_POINT('',(-387.309362287183,-429.052084029138,-209.824281504696));
#32245=CARTESIAN_POINT('',(-387.309362287183,-429.052084029138,-209.824281504696));
#32246=CARTESIAN_POINT('',(-376.048949668551,-423.426014040814,-213.072426228171));
#32247=CARTESIAN_POINT('',(-376.048949668551,-423.426014040814,-213.072426228171));
#32248=CARTESIAN_POINT('',(-376.048949668551,-423.426014040814,-213.072426228171));
#32249=CARTESIAN_POINT('Origin',(-376.048949668551,-533.224282489496,-403.252604600343));
#32250=CARTESIAN_POINT('',(-387.309362287183,-538.85035247782,-400.004459876868));
#32251=CARTESIAN_POINT('',(-376.048949668551,-533.224282489496,-403.252604600343));
#32252=CARTESIAN_POINT('Origin',(-394.754129766534,-197.232058670006,113.869587829266));
#32253=CARTESIAN_POINT('Origin',(-406.014542385166,-202.85812865833,117.117732552741));
#32254=CARTESIAN_POINT('Origin',(-376.051116910575,-418.422839624243,-204.414004948869));
#32255=CARTESIAN_POINT('',(-387.311529529207,-424.048909612567,-201.165860225394));
#32256=CARTESIAN_POINT('',(-328.344280017437,-512.565744095532,-150.061716576057));
#32257=CARTESIAN_POINT('',(-387.311529529207,-424.048909612567,-201.165860225394));
#32258=CARTESIAN_POINT('',(-376.051116910575,-418.422839624243,-204.414004948869));
#32259=CARTESIAN_POINT('',(-376.051116910575,-418.422839624243,-204.414004948869));
#32260=CARTESIAN_POINT('',(-317.083867398805,-506.939674107208,-153.309861299531));
#32261=CARTESIAN_POINT('',(-376.051116910575,-418.422839624243,-204.414004948869));
#32262=CARTESIAN_POINT('',(-317.083867398805,-506.939674107208,-153.309861299531));
#32263=CARTESIAN_POINT('Origin',(-317.083867398805,-506.939674107208,-153.309861299531));
#32264=CARTESIAN_POINT('',(-328.344280017437,-402.76747564685,40.1184617961154));
#32265=CARTESIAN_POINT('',(-328.344280017437,-512.565744095532,-150.061716576057));
#32266=CARTESIAN_POINT('',(-317.083867398805,-397.141405658526,36.8703170726406));
#32267=CARTESIAN_POINT('',(-317.083867398805,-506.939674107208,-153.309861299531));
#32268=CARTESIAN_POINT('',(-317.083867398805,-397.141405658526,36.8703170726406));
#32269=CARTESIAN_POINT('Origin',(-376.051116910575,-308.624571175561,-14.2338265766968));
#32270=CARTESIAN_POINT('',(-387.311529529207,-314.250641163885,-10.985681853222));
#32271=CARTESIAN_POINT('',(-387.311529529207,-314.250641163885,-10.985681853222));
#32272=CARTESIAN_POINT('',(-376.051116910575,-308.624571175561,-14.2338265766968));
#32273=CARTESIAN_POINT('',(-376.051116910575,-308.624571175561,-14.2338265766968));
#32274=CARTESIAN_POINT('',(-376.051116910575,-308.624571175561,-14.2338265766968));
#32275=CARTESIAN_POINT('Origin',(-376.051116910575,-418.422839624243,-204.414004948869));
#32276=CARTESIAN_POINT('',(-387.311529529207,-424.048909612567,-201.165860225394));
#32277=CARTESIAN_POINT('',(-376.051116910575,-418.422839624243,-204.414004948869));
#32278=CARTESIAN_POINT('Origin',(-394.756297008558,-82.4306158047535,312.70818748074));
#32279=CARTESIAN_POINT('Origin',(-406.016709627189,-88.0566857930775,315.956332204215));
#32280=CARTESIAN_POINT('Origin',(-312.084475633296,-629.241334735898,-347.815507460388));
#32281=CARTESIAN_POINT('',(-323.344888251928,-634.867404724222,-344.567362736913));
#32282=CARTESIAN_POINT('',(-264.377638740158,-723.384239207187,-293.463219087576));
#32283=CARTESIAN_POINT('',(-323.344888251928,-634.867404724222,-344.567362736913));
#32284=CARTESIAN_POINT('',(-312.084475633296,-629.241334735898,-347.815507460388));
#32285=CARTESIAN_POINT('',(-312.084475633296,-629.241334735898,-347.815507460388));
#32286=CARTESIAN_POINT('',(-253.117226121526,-717.758169218862,-296.711363811051));
#32287=CARTESIAN_POINT('',(-312.084475633296,-629.241334735898,-347.815507460388));
#32288=CARTESIAN_POINT('',(-253.117226121526,-717.758169218862,-296.711363811051));
#32289=CARTESIAN_POINT('Origin',(-253.117226121526,-717.758169218862,-296.711363811051));
#32290=CARTESIAN_POINT('',(-264.377638740158,-613.585970758505,-103.283040715404));
#32291=CARTESIAN_POINT('',(-264.377638740158,-723.384239207187,-293.463219087576));
#32292=CARTESIAN_POINT('',(-253.117226121526,-607.959900770181,-106.531185438879));
#32293=CARTESIAN_POINT('',(-253.117226121526,-717.758169218862,-296.711363811051));
#32294=CARTESIAN_POINT('',(-253.117226121526,-607.959900770181,-106.531185438879));
#32295=CARTESIAN_POINT('Origin',(-312.084475633296,-519.443066287216,-157.635329088216));
#32296=CARTESIAN_POINT('',(-323.344888251928,-525.06913627554,-154.387184364741));
#32297=CARTESIAN_POINT('',(-323.344888251928,-525.06913627554,-154.387184364741));
#32298=CARTESIAN_POINT('',(-312.084475633296,-519.443066287216,-157.635329088216));
#32299=CARTESIAN_POINT('',(-312.084475633296,-519.443066287216,-157.635329088216));
#32300=CARTESIAN_POINT('',(-312.084475633296,-519.443066287216,-157.635329088216));
#32301=CARTESIAN_POINT('Origin',(-312.084475633296,-629.241334735898,-347.815507460388));
#32302=CARTESIAN_POINT('',(-323.344888251928,-634.867404724222,-344.567362736913));
#32303=CARTESIAN_POINT('',(-312.084475633296,-629.241334735898,-347.815507460388));
#32304=CARTESIAN_POINT('Origin',(-330.789655731279,-293.249110916408,169.306684969221));
#32305=CARTESIAN_POINT('Origin',(-342.050068349911,-298.875180904732,172.554829692696));
#32306=CARTESIAN_POINT('Origin',(-312.08664287532,-514.439891870646,-148.976907808914));
#32307=CARTESIAN_POINT('',(-323.347055493952,-520.06596185897,-145.728763085439));
#32308=CARTESIAN_POINT('',(-264.379805982182,-608.582796341934,-94.6246194361014));
#32309=CARTESIAN_POINT('',(-323.347055493952,-520.06596185897,-145.728763085439));
#32310=CARTESIAN_POINT('',(-312.08664287532,-514.439891870646,-148.976907808914));
#32311=CARTESIAN_POINT('',(-312.08664287532,-514.439891870646,-148.976907808914));
#32312=CARTESIAN_POINT('',(-253.11939336355,-602.95672635361,-97.8727641595762));
#32313=CARTESIAN_POINT('',(-312.08664287532,-514.439891870646,-148.976907808914));
#32314=CARTESIAN_POINT('',(-253.11939336355,-602.95672635361,-97.8727641595762));
#32315=CARTESIAN_POINT('Origin',(-253.11939336355,-602.95672635361,-97.8727641595762));
#32316=CARTESIAN_POINT('',(-264.379805982182,-498.784527893252,95.5555589360706));
#32317=CARTESIAN_POINT('',(-264.379805982182,-608.582796341934,-94.6246194361014));
#32318=CARTESIAN_POINT('',(-253.11939336355,-493.158457904928,92.3074142125958));
#32319=CARTESIAN_POINT('',(-253.11939336355,-602.95672635361,-97.8727641595762));
#32320=CARTESIAN_POINT('',(-253.11939336355,-493.158457904928,92.3074142125958));
#32321=CARTESIAN_POINT('Origin',(-312.08664287532,-404.641623421964,41.2032705632584));
#32322=CARTESIAN_POINT('',(-323.347055493952,-410.267693410288,44.4514152867332));
#32323=CARTESIAN_POINT('',(-323.347055493952,-410.267693410288,44.4514152867332));
#32324=CARTESIAN_POINT('',(-312.08664287532,-404.641623421964,41.2032705632584));
#32325=CARTESIAN_POINT('',(-312.08664287532,-404.641623421964,41.2032705632584));
#32326=CARTESIAN_POINT('',(-312.08664287532,-404.641623421964,41.2032705632584));
#32327=CARTESIAN_POINT('Origin',(-312.08664287532,-514.439891870646,-148.976907808914));
#32328=CARTESIAN_POINT('',(-323.347055493952,-520.06596185897,-145.728763085439));
#32329=CARTESIAN_POINT('',(-312.08664287532,-514.439891870646,-148.976907808914));
#32330=CARTESIAN_POINT('Origin',(-330.791822973303,-178.447668051156,368.145284620695));
#32331=CARTESIAN_POINT('Origin',(-342.052235591935,-184.07373803948,371.39342934417));
#32332=CARTESIAN_POINT('Origin',(368.833006272647,-291.775764149142,-9.65537551417994));
#32333=CARTESIAN_POINT('',(368.833128982344,-285.27568245381,1.60290756713166));
#32334=CARTESIAN_POINT('',(-368.828409446333,-285.27220098925,1.60893765350545));
#32335=CARTESIAN_POINT('',(368.833128982344,-285.27568245381,1.60290756713166));
#32336=CARTESIAN_POINT('',(368.833006272647,-291.775764149142,-9.65537551417994));
#32337=CARTESIAN_POINT('',(368.833006272647,-291.775764149142,-9.65537551417994));
#32338=CARTESIAN_POINT('',(-368.828532156029,-291.772282684582,-9.64934542780627));
#32339=CARTESIAN_POINT('',(368.833006272647,-291.775764149142,-9.65537551417994));
#32340=CARTESIAN_POINT('',(-368.828532156029,-291.772282684582,-9.64934542780627));
#32341=CARTESIAN_POINT('Origin',(-368.828532156029,-291.772282684582,-9.64934542780627));
#32342=CARTESIAN_POINT('',(-201.635208823479,-536.24744098009,146.510165970204));
#32343=CARTESIAN_POINT('',(-368.828409446333,-285.27220098925,1.60893765350545));
#32344=CARTESIAN_POINT('',(-201.635331533176,-542.747522675422,135.251882888892));
#32345=CARTESIAN_POINT('',(-368.828532156029,-291.772282684582,-9.64934542780627));
#32346=CARTESIAN_POINT('',(-201.635331533176,-542.747522675422,135.251882888892));
#32347=CARTESIAN_POINT('Origin',(-201.635331533176,-542.747522675422,135.251882888892));
#32348=CARTESIAN_POINT('',(201.639928404246,-536.249344275877,146.506869358163));
#32349=CARTESIAN_POINT('',(-201.635208823479,-536.24744098009,146.510165970204));
#32350=CARTESIAN_POINT('',(201.63980569455,-542.74942597121,135.248586276851));
#32351=CARTESIAN_POINT('',(-201.635331533176,-542.747522675422,135.251882888892));
#32352=CARTESIAN_POINT('',(201.63980569455,-542.74942597121,135.248586276851));
#32353=CARTESIAN_POINT('Origin',(201.63980569455,-542.74942597121,135.248586276851));
#32354=CARTESIAN_POINT('',(201.639928404246,-536.249344275877,146.506869358163));
#32355=CARTESIAN_POINT('',(201.63980569455,-542.74942597121,135.248586276851));
#32356=CARTESIAN_POINT('Origin',(0.0022370391692238,-77.1194255571307,-133.585327184455));
#32357=CARTESIAN_POINT('Origin',(0.00235974886567285,-70.6193438617984,
-122.327044103143));
#32358=CARTESIAN_POINT('Origin',(374.6,62.3000000000001,-13.));
#32359=CARTESIAN_POINT('',(374.6,62.3000000000001,0.));
#32360=CARTESIAN_POINT('',(374.6,-267.5,0.));
#32361=CARTESIAN_POINT('',(374.6,62.3000000000001,0.));
#32362=CARTESIAN_POINT('',(374.6,-267.5,-13.));
#32363=CARTESIAN_POINT('',(374.6,-267.5,-13.));
#32364=CARTESIAN_POINT('',(374.6,62.3000000000001,-13.));
#32365=CARTESIAN_POINT('',(374.6,62.3000000000001,-13.));
#32366=CARTESIAN_POINT('',(374.6,62.3000000000001,-13.));
#32367=CARTESIAN_POINT('Origin',(374.6,-267.5,-13.));
#32368=CARTESIAN_POINT('',(194.8,-267.5,0.));
#32369=CARTESIAN_POINT('',(374.6,-267.5,0.));
#32370=CARTESIAN_POINT('',(194.8,-267.5,-13.));
#32371=CARTESIAN_POINT('',(194.8,-267.5,-13.));
#32372=CARTESIAN_POINT('',(374.6,-267.5,-13.));
#32373=CARTESIAN_POINT('Origin',(194.8,62.3000000000001,-13.));
#32374=CARTESIAN_POINT('',(194.8,62.3000000000001,0.));
#32375=CARTESIAN_POINT('',(194.8,62.3000000000001,0.));
#32376=CARTESIAN_POINT('',(194.8,62.3000000000001,-13.));
#32377=CARTESIAN_POINT('',(194.8,62.3000000000001,-13.));
#32378=CARTESIAN_POINT('',(194.8,62.3000000000001,-13.));
#32379=CARTESIAN_POINT('Origin',(374.6,62.3000000000001,-13.));
#32380=CARTESIAN_POINT('',(374.6,62.3000000000001,0.));
#32381=CARTESIAN_POINT('',(374.6,62.3000000000001,-13.));
#32382=CARTESIAN_POINT('Origin',(0.,0.,-13.));
#32383=CARTESIAN_POINT('Origin',(0.,0.,0.));
#32384=CARTESIAN_POINT('Origin',(184.8,62.3000000000001,-13.));
#32385=CARTESIAN_POINT('',(184.8,62.3000000000001,0.));
#32386=CARTESIAN_POINT('',(184.8,-267.5,0.));
#32387=CARTESIAN_POINT('',(184.8,62.3000000000001,0.));
#32388=CARTESIAN_POINT('',(184.8,-267.5,-13.));
#32389=CARTESIAN_POINT('',(184.8,-267.5,-13.));
#32390=CARTESIAN_POINT('',(184.8,62.3000000000001,-13.));
#32391=CARTESIAN_POINT('',(184.8,62.3000000000001,-13.));
#32392=CARTESIAN_POINT('',(184.8,62.3000000000001,-13.));
#32393=CARTESIAN_POINT('Origin',(184.8,-267.5,-13.));
#32394=CARTESIAN_POINT('',(4.99999999999998,-267.5,0.));
#32395=CARTESIAN_POINT('',(184.8,-267.5,0.));
#32396=CARTESIAN_POINT('',(4.99999999999998,-267.5,-13.));
#32397=CARTESIAN_POINT('',(4.99999999999998,-267.5,-13.));
#32398=CARTESIAN_POINT('',(184.8,-267.5,-13.));
#32399=CARTESIAN_POINT('Origin',(5.00000000000003,62.3000000000001,-13.));
#32400=CARTESIAN_POINT('',(5.00000000000003,62.3000000000001,0.));
#32401=CARTESIAN_POINT('',(5.00000000000003,62.3000000000001,0.));
#32402=CARTESIAN_POINT('',(5.00000000000003,62.3000000000001,-13.));
#32403=CARTESIAN_POINT('',(5.00000000000003,62.3000000000001,-13.));
#32404=CARTESIAN_POINT('',(5.00000000000003,62.3000000000001,-13.));
#32405=CARTESIAN_POINT('Origin',(184.8,62.3000000000001,-13.));
#32406=CARTESIAN_POINT('',(184.8,62.3000000000001,0.));
#32407=CARTESIAN_POINT('',(184.8,62.3000000000001,-13.));
#32408=CARTESIAN_POINT('Origin',(0.,0.,-13.));
#32409=CARTESIAN_POINT('Origin',(0.,0.,0.));
#32410=CARTESIAN_POINT('Origin',(374.6,72.3000000000001,-13.));
#32411=CARTESIAN_POINT('',(374.6,252.1,0.));
#32412=CARTESIAN_POINT('',(374.6,72.3000000000001,0.));
#32413=CARTESIAN_POINT('',(374.6,72.3000000000001,0.));
#32414=CARTESIAN_POINT('',(374.6,72.3000000000001,-13.));
#32415=CARTESIAN_POINT('',(374.6,72.3000000000001,-13.));
#32416=CARTESIAN_POINT('',(374.6,252.1,-13.));
#32417=CARTESIAN_POINT('',(374.6,72.3000000000001,-13.));
#32418=CARTESIAN_POINT('',(374.6,252.1,-13.));
#32419=CARTESIAN_POINT('Origin',(374.6,72.3000000000001,-13.));
#32420=CARTESIAN_POINT('',(5.,72.3000000000001,0.));
#32421=CARTESIAN_POINT('',(374.6,72.3000000000001,0.));
#32422=CARTESIAN_POINT('',(5.,72.3000000000001,-13.));
#32423=CARTESIAN_POINT('',(5.,72.3000000000001,-13.));
#32424=CARTESIAN_POINT('',(374.6,72.3000000000001,-13.));
#32425=CARTESIAN_POINT('Origin',(5.,72.3000000000001,-13.));
#32426=CARTESIAN_POINT('',(5.,252.1,0.));
#32427=CARTESIAN_POINT('',(5.,72.3000000000001,0.));
#32428=CARTESIAN_POINT('',(5.,252.1,-13.));
#32429=CARTESIAN_POINT('',(5.,252.1,-13.));
#32430=CARTESIAN_POINT('',(5.,72.3000000000001,-13.));
#32431=CARTESIAN_POINT('Origin',(374.6,252.1,-13.));
#32432=CARTESIAN_POINT('',(374.6,252.1,0.));
#32433=CARTESIAN_POINT('',(374.6,252.1,-13.));
#32434=CARTESIAN_POINT('Origin',(0.,0.,-13.));
#32435=CARTESIAN_POINT('Origin',(0.,0.,0.));
#32436=CARTESIAN_POINT('Origin',(-5.,72.3000000000001,-13.));
#32437=CARTESIAN_POINT('',(-5.,252.1,0.));
#32438=CARTESIAN_POINT('',(-5.,72.3000000000001,0.));
#32439=CARTESIAN_POINT('',(-5.,72.3000000000001,0.));
#32440=CARTESIAN_POINT('',(-5.,72.3000000000001,-13.));
#32441=CARTESIAN_POINT('',(-5.,72.3000000000001,-13.));
#32442=CARTESIAN_POINT('',(-5.,252.1,-13.));
#32443=CARTESIAN_POINT('',(-5.,72.3000000000001,-13.));
#32444=CARTESIAN_POINT('',(-5.,252.1,-13.));
#32445=CARTESIAN_POINT('Origin',(-5.,72.3000000000001,-13.));
#32446=CARTESIAN_POINT('',(-374.6,72.3000000000001,0.));
#32447=CARTESIAN_POINT('',(-5.,72.3000000000001,0.));
#32448=CARTESIAN_POINT('',(-374.6,72.3000000000001,-13.));
#32449=CARTESIAN_POINT('',(-374.6,72.3000000000001,-13.));
#32450=CARTESIAN_POINT('',(-5.,72.3000000000001,-13.));
#32451=CARTESIAN_POINT('Origin',(-374.6,72.3000000000001,-13.));
#32452=CARTESIAN_POINT('',(-374.6,252.1,0.));
#32453=CARTESIAN_POINT('',(-374.6,72.3000000000001,0.));
#32454=CARTESIAN_POINT('',(-374.6,252.1,-13.));
#32455=CARTESIAN_POINT('',(-374.6,252.1,-13.));
#32456=CARTESIAN_POINT('',(-374.6,72.3000000000001,-13.));
#32457=CARTESIAN_POINT('Origin',(-5.,252.1,-13.));
#32458=CARTESIAN_POINT('',(-5.,252.1,0.));
#32459=CARTESIAN_POINT('',(-5.,252.1,-13.));
#32460=CARTESIAN_POINT('Origin',(0.,0.,-13.));
#32461=CARTESIAN_POINT('Origin',(0.,0.,0.));
#32462=CARTESIAN_POINT('Origin',(-4.99999999999989,62.3000000000001,-13.));
#32463=CARTESIAN_POINT('',(-4.99999999999989,62.3000000000001,0.));
#32464=CARTESIAN_POINT('',(-5.00000000000002,-267.5,0.));
#32465=CARTESIAN_POINT('',(-4.99999999999989,62.3000000000001,0.));
#32466=CARTESIAN_POINT('',(-5.00000000000002,-267.5,-13.));
#32467=CARTESIAN_POINT('',(-5.00000000000002,-267.5,-13.));
#32468=CARTESIAN_POINT('',(-4.99999999999989,62.3000000000001,-13.));
#32469=CARTESIAN_POINT('',(-4.99999999999989,62.3000000000001,-13.));
#32470=CARTESIAN_POINT('',(-4.99999999999989,62.3000000000001,-13.));
#32471=CARTESIAN_POINT('Origin',(-5.00000000000002,-267.5,-13.));
#32472=CARTESIAN_POINT('',(-184.8,-267.5,0.));
#32473=CARTESIAN_POINT('',(-5.00000000000002,-267.5,0.));
#32474=CARTESIAN_POINT('',(-184.8,-267.5,-13.));
#32475=CARTESIAN_POINT('',(-184.8,-267.5,-13.));
#32476=CARTESIAN_POINT('',(-5.00000000000002,-267.5,-13.));
#32477=CARTESIAN_POINT('Origin',(-184.8,62.3000000000001,-13.));
#32478=CARTESIAN_POINT('',(-184.8,62.3000000000001,0.));
#32479=CARTESIAN_POINT('',(-184.8,62.3000000000001,0.));
#32480=CARTESIAN_POINT('',(-184.8,62.3000000000001,-13.));
#32481=CARTESIAN_POINT('',(-184.8,62.3000000000001,-13.));
#32482=CARTESIAN_POINT('',(-184.8,62.3000000000001,-13.));
#32483=CARTESIAN_POINT('Origin',(-4.99999999999989,62.3000000000001,-13.));
#32484=CARTESIAN_POINT('',(-4.99999999999989,62.3000000000001,0.));
#32485=CARTESIAN_POINT('',(-4.99999999999989,62.3000000000001,-13.));
#32486=CARTESIAN_POINT('Origin',(0.,0.,-13.));
#32487=CARTESIAN_POINT('Origin',(0.,0.,0.));
#32488=CARTESIAN_POINT('Origin',(-194.8,62.3000000000001,-13.));
#32489=CARTESIAN_POINT('',(-194.8,62.3000000000001,0.));
#32490=CARTESIAN_POINT('',(-194.8,-267.5,0.));
#32491=CARTESIAN_POINT('',(-194.8,62.3000000000001,0.));
#32492=CARTESIAN_POINT('',(-194.8,-267.5,-13.));
#32493=CARTESIAN_POINT('',(-194.8,-267.5,-13.));
#32494=CARTESIAN_POINT('',(-194.8,62.3000000000001,-13.));
#32495=CARTESIAN_POINT('',(-194.8,62.3000000000001,-13.));
#32496=CARTESIAN_POINT('',(-194.8,62.3000000000001,-13.));
#32497=CARTESIAN_POINT('Origin',(-194.8,-267.5,-13.));
#32498=CARTESIAN_POINT('',(-374.6,-267.5,0.));
#32499=CARTESIAN_POINT('',(-194.8,-267.5,0.));
#32500=CARTESIAN_POINT('',(-374.6,-267.5,-13.));
#32501=CARTESIAN_POINT('',(-374.6,-267.5,-13.));
#32502=CARTESIAN_POINT('',(-194.8,-267.5,-13.));
#32503=CARTESIAN_POINT('Origin',(-374.6,62.3000000000001,-13.));
#32504=CARTESIAN_POINT('',(-374.6,62.3000000000001,0.));
#32505=CARTESIAN_POINT('',(-374.6,62.3000000000001,0.));
#32506=CARTESIAN_POINT('',(-374.6,62.3000000000001,-13.));
#32507=CARTESIAN_POINT('',(-374.6,62.3000000000001,-13.));
#32508=CARTESIAN_POINT('',(-374.6,62.3000000000001,-13.));
#32509=CARTESIAN_POINT('Origin',(-194.8,62.3000000000001,-13.));
#32510=CARTESIAN_POINT('',(-194.8,62.3000000000001,0.));
#32511=CARTESIAN_POINT('',(-194.8,62.3000000000001,-13.));
#32512=CARTESIAN_POINT('Origin',(0.,0.,-13.));
#32513=CARTESIAN_POINT('Origin',(0.,0.,0.));
#32514=CARTESIAN_POINT('',(0.,0.,0.));
#32515=CARTESIAN_POINT('Origin',(11.2,0.,0.));
#32516=CARTESIAN_POINT('',(11.2,9.79717439317883E-16,-8.));
#32517=CARTESIAN_POINT('',(11.2,-9.79717439317883E-16,8.));
#32518=CARTESIAN_POINT('Origin',(11.2,0.,0.));
#32519=CARTESIAN_POINT('Origin',(11.2,0.,0.));
#32520=CARTESIAN_POINT('',(10.,-1.12667505521557E-15,9.2));
#32521=CARTESIAN_POINT('Origin',(11.2,-1.12667505521557E-15,9.2));
#32522=CARTESIAN_POINT('Origin',(10.,0.,0.));
#32523=CARTESIAN_POINT('Origin',(0.,0.,0.));
#32524=CARTESIAN_POINT('',(9.4,-11.6913429510899,6.75000000000002));
#32525=CARTESIAN_POINT('',(9.4,0.,13.5));
#32526=CARTESIAN_POINT('Origin',(9.4,0.,0.));
#32527=CARTESIAN_POINT('',(9.4,-11.6913429510899,-6.75));
#32528=CARTESIAN_POINT('Origin',(9.4,0.,0.));
#32529=CARTESIAN_POINT('',(9.4,3.00462919747432E-15,-13.5));
#32530=CARTESIAN_POINT('Origin',(9.4,0.,0.));
#32531=CARTESIAN_POINT('',(10.,-1.65327317884893E-15,-13.5));
#32532=CARTESIAN_POINT('',(0.,-1.65327317884893E-15,-13.5));
#32533=CARTESIAN_POINT('Origin',(10.,0.,0.));
#32534=CARTESIAN_POINT('',(9.4,11.6913429510899,-6.75000000000001));
#32535=CARTESIAN_POINT('Origin',(9.4,0.,0.));
#32536=CARTESIAN_POINT('',(9.4,11.6913429510899,6.75000000000001));
#32537=CARTESIAN_POINT('Origin',(9.4,0.,0.));
#32538=CARTESIAN_POINT('Origin',(9.4,0.,0.));
#32539=CARTESIAN_POINT('Origin',(70.,0.,0.));
#32540=CARTESIAN_POINT('',(68.8985,-9.79717439317882E-16,-8.));
#32541=CARTESIAN_POINT('Origin',(68.8985,0.,0.));
#32542=CARTESIAN_POINT('',(70.,-8.44822594391802E-16,-6.8985));
#32543=CARTESIAN_POINT('',(70.,-8.44822594391802E-16,-6.8985));
#32544=CARTESIAN_POINT('Origin',(70.,0.,0.));
#32545=CARTESIAN_POINT('Origin',(0.,0.,0.));
#32546=CARTESIAN_POINT('',(0.,-9.79717439317883E-16,-8.));
#32547=CARTESIAN_POINT('Origin',(10.,15.5884572681199,-1.3010426069826E-15));
#32548=CARTESIAN_POINT('Origin',(70.,0.,0.));
#32549=CARTESIAN_POINT('Origin',(9.4,13.5,0.));
#32550=CARTESIAN_POINT('',(9.4,7.79422863405994,-13.5));
#32551=CARTESIAN_POINT('',(9.4,7.79422863405994,-13.5));
#32552=CARTESIAN_POINT('',(9.4,7.79422863405994,-13.5));
#32553=CARTESIAN_POINT('Origin',(9.4,13.5,0.));
#32554=CARTESIAN_POINT('',(9.4,15.5884572681199,0.));
#32555=CARTESIAN_POINT('',(9.4,7.79422863405994,-13.5));
#32556=CARTESIAN_POINT('',(9.4,15.5884572681199,0.));
#32557=CARTESIAN_POINT('Origin',(9.4,13.5,0.));
#32558=CARTESIAN_POINT('',(9.4,7.79422863405994,13.5));
#32559=CARTESIAN_POINT('',(9.4,15.5884572681199,0.));
#32560=CARTESIAN_POINT('',(9.4,7.79422863405994,13.5));
#32561=CARTESIAN_POINT('Origin',(9.4,13.5,0.));
#32562=CARTESIAN_POINT('',(9.4,-7.79422863405994,13.5));
#32563=CARTESIAN_POINT('',(9.4,7.79422863405994,13.5));
#32564=CARTESIAN_POINT('',(9.4,-15.5884572681199,8.77615707241165E-17));
#32565=CARTESIAN_POINT('Origin',(9.4,13.5,0.));
#32566=CARTESIAN_POINT('',(9.4,-15.5884572681199,0.));
#32567=CARTESIAN_POINT('',(9.4,-15.5884572681199,8.77615707241165E-17));
#32568=CARTESIAN_POINT('',(9.4,-7.79422863405996,-13.5));
#32569=CARTESIAN_POINT('Origin',(9.4,13.5,0.));
#32570=CARTESIAN_POINT('',(9.4,-7.79422863405996,-13.5));
#32571=CARTESIAN_POINT('',(9.4,-7.79422863405996,-13.5));
#32572=CARTESIAN_POINT('',(9.4,7.79422863405994,-13.5));
#32573=CARTESIAN_POINT('Origin',(0.,15.5884572681199,-1.3010426069826E-15));
#32574=CARTESIAN_POINT('',(0.,3.00462919747432E-15,-13.5));
#32575=CARTESIAN_POINT('',(0.,11.6913429510899,-6.75000000000001));
#32576=CARTESIAN_POINT('Origin',(0.,0.,0.));
#32577=CARTESIAN_POINT('',(0.,-11.6913429510899,-6.75));
#32578=CARTESIAN_POINT('Origin',(0.,0.,0.));
#32579=CARTESIAN_POINT('',(0.,-11.6913429510899,6.75000000000001));
#32580=CARTESIAN_POINT('Origin',(0.,0.,0.));
#32581=CARTESIAN_POINT('',(0.,3.00462919747432E-15,13.5));
#32582=CARTESIAN_POINT('Origin',(0.,0.,0.));
#32583=CARTESIAN_POINT('',(0.,11.6913429510899,6.75000000000001));
#32584=CARTESIAN_POINT('Origin',(0.,0.,0.));
#32585=CARTESIAN_POINT('Origin',(0.,0.,0.));
#32586=CARTESIAN_POINT('Origin',(0.,0.,0.));
#32587=CARTESIAN_POINT('',(1.20577136594005,15.5884572681199,1.14068201043699E-16));
#32588=CARTESIAN_POINT('Ctrl Pts',(7.99123887912295E-16,11.6913429510899,
6.75000000000001));
#32589=CARTESIAN_POINT('Ctrl Pts',(2.44249065417534E-15,13.5000000000004,
3.61731409781943));
#32590=CARTESIAN_POINT('Ctrl Pts',(1.20577136594065,15.5884572681209,-1.81141005043525E-12));
#32591=CARTESIAN_POINT('Ctrl Pts',(1.20577136594066,15.588457268121,1.8228892015787E-12));
#32592=CARTESIAN_POINT('Ctrl Pts',(3.6583932433027E-15,13.5000000000004,
-3.61731409781942));
#32593=CARTESIAN_POINT('Ctrl Pts',(7.99123887912298E-16,11.6913429510899,
-6.75));
#32594=CARTESIAN_POINT('Origin',(0.,0.,0.));
#32595=CARTESIAN_POINT('',(1.20577136594004,7.79422863405994,13.5));
#32596=CARTESIAN_POINT('Ctrl Pts',(2.66374629304099E-16,-1.06549851721639E-15,
13.5));
#32597=CARTESIAN_POINT('Ctrl Pts',(-6.66133814775094E-16,3.617314097821,
13.5));
#32598=CARTESIAN_POINT('Ctrl Pts',(1.20577136594065,7.79422863406204,13.5));
#32599=CARTESIAN_POINT('Ctrl Pts',(1.20577136594064,7.7942286340589,13.5000000000018));
#32600=CARTESIAN_POINT('Ctrl Pts',(-6.67981053492038E-16,9.88268590217942,
9.88268590218058));
#32601=CARTESIAN_POINT('Ctrl Pts',(7.99123887912295E-16,11.6913429510899,
6.75000000000001));
#32602=CARTESIAN_POINT('Origin',(0.,0.,0.));
#32603=CARTESIAN_POINT('',(1.20577136594004,-7.79422863405994,13.5));
#32604=CARTESIAN_POINT('Ctrl Pts',(1.20577136594065,-7.79422863406204,13.5));
#32605=CARTESIAN_POINT('Ctrl Pts',(1.09406226090395E-15,-3.617314097821,
13.5));
#32606=CARTESIAN_POINT('Ctrl Pts',(2.66374629304099E-16,-1.06549851721639E-15,
13.5));
#32607=CARTESIAN_POINT('Ctrl Pts',(3.19649555164917E-15,-11.6913429510899,
6.75000000000002));
#32608=CARTESIAN_POINT('Ctrl Pts',(3.44169137633799E-15,-9.88268590217941,
9.88268590218058));
#32609=CARTESIAN_POINT('Ctrl Pts',(1.20577136594065,-7.79422863405889,13.5000000000018));
#32610=CARTESIAN_POINT('Origin',(0.,0.,0.));
#32611=CARTESIAN_POINT('',(1.20577136594005,-15.5884572681199,1.05679326596683E-16));
#32612=CARTESIAN_POINT('Ctrl Pts',(1.20577136594066,-15.588457268121,-1.82403711669304E-12));
#32613=CARTESIAN_POINT('Ctrl Pts',(3.15927592518995E-15,-13.5000000000004,
3.61731409781943));
#32614=CARTESIAN_POINT('Ctrl Pts',(3.19649555164917E-15,-11.6913429510899,
6.75000000000002));
#32615=CARTESIAN_POINT('Ctrl Pts',(5.59386721538605E-15,-11.6913429510899,
-6.75000000000001));
#32616=CARTESIAN_POINT('Ctrl Pts',(4.77395900588817E-15,-13.5000000000004,
-3.61731409781943));
#32617=CARTESIAN_POINT('Ctrl Pts',(1.20577136594065,-15.5884572681209,1.8062444324207E-12));
#32618=CARTESIAN_POINT('Origin',(0.,0.,0.));
#32619=CARTESIAN_POINT('',(1.20577136594004,7.79422863405994,-13.5));
#32620=CARTESIAN_POINT('Ctrl Pts',(7.99123887912298E-16,11.6913429510899,
-6.75));
#32621=CARTESIAN_POINT('Ctrl Pts',(-1.88737914186277E-15,9.88268590217942,
-9.88268590218057));
#32622=CARTESIAN_POINT('Ctrl Pts',(1.20577136594065,7.79422863405889,-13.5000000000018));
#32623=CARTESIAN_POINT('Ctrl Pts',(1.20577136594065,7.79422863406204,-13.5));
#32624=CARTESIAN_POINT('Ctrl Pts',(-9.97494936421185E-17,3.61731409782101,
-13.5));
#32625=CARTESIAN_POINT('Ctrl Pts',(-2.13099703443277E-15,2.02444718271114E-14,
-13.5));
#32626=CARTESIAN_POINT('Origin',(0.,0.,0.));
#32627=CARTESIAN_POINT('',(1.20577136594005,-7.79422863405996,-13.5));
#32628=CARTESIAN_POINT('Ctrl Pts',(1.20577136594065,-7.79422863405891,-13.5000000000018));
#32629=CARTESIAN_POINT('Ctrl Pts',(6.79842967357653E-15,-9.88268590217943,
-9.88268590218058));
#32630=CARTESIAN_POINT('Ctrl Pts',(5.59386721538605E-15,-11.6913429510899,
-6.75000000000001));
#32631=CARTESIAN_POINT('Ctrl Pts',(-2.13099703443277E-15,2.02444718271114E-14,
-13.5));
#32632=CARTESIAN_POINT('Ctrl Pts',(-4.77395900588817E-15,-3.61731409782099,
-13.5));
#32633=CARTESIAN_POINT('Ctrl Pts',(1.20577136594065,-7.79422863406205,-13.5));
#32634=CARTESIAN_POINT('Origin',(10.,7.79422863405994,-13.5));
#32635=CARTESIAN_POINT('',(10.,-7.79422863405996,-13.5));
#32636=CARTESIAN_POINT('',(10.,7.79422863405994,-13.5));
#32637=CARTESIAN_POINT('Origin',(10.,-7.79422863405996,-13.5));
#32638=CARTESIAN_POINT('',(10.,-15.5884572681199,8.77615707241165E-17));
#32639=CARTESIAN_POINT('Origin',(10.,-15.5884572681199,8.77615707241165E-17));
#32640=CARTESIAN_POINT('',(10.,-7.79422863405994,13.5));
#32641=CARTESIAN_POINT('Origin',(10.,7.79422863405994,13.5));
#32642=CARTESIAN_POINT('',(10.,7.79422863405994,13.5));
#32643=CARTESIAN_POINT('Origin',(10.,15.5884572681199,0.));
#32644=CARTESIAN_POINT('',(10.,15.5884572681199,0.));
#32645=CARTESIAN_POINT('Origin',(10.,7.79422863405994,-13.5));
#32646=CARTESIAN_POINT('',(0.,0.,0.));
#32647=CARTESIAN_POINT('Origin',(-34.9249999999999,0.,0.));
#32648=CARTESIAN_POINT('',(-2.99999999999999,-1.83697019872103E-15,-15.));
#32649=CARTESIAN_POINT('Origin',(-3.,0.,0.));
#32650=CARTESIAN_POINT('',(4.44089209850063E-15,-1.83697019872103E-15,-15.));
#32651=CARTESIAN_POINT('',(-34.9249999999999,-1.83697019872103E-15,-15.));
#32652=CARTESIAN_POINT('Origin',(0.,0.,0.));
#32653=CARTESIAN_POINT('Origin',(-34.9249999999999,0.,0.));
#32654=CARTESIAN_POINT('',(-4.44089209850063E-15,-1.04094977927525E-15,
-8.49999999999999));
#32655=CARTESIAN_POINT('Origin',(0.,0.,0.));
#32656=CARTESIAN_POINT('',(-2.99999999999999,-1.04094977927525E-15,-8.49999999999999));
#32657=CARTESIAN_POINT('',(-34.9249999999999,-1.04094977927525E-15,-8.49999999999999));
#32658=CARTESIAN_POINT('Origin',(-3.,0.,0.));
#32659=CARTESIAN_POINT('Origin',(0.,8.49999999999999,0.));
#32660=CARTESIAN_POINT('Origin',(-3.,15.,0.));
#32661=CARTESIAN_POINT('',(0.,0.,0.));
#32662=CARTESIAN_POINT('Origin',(0.,0.,-25.0375057290932));
#32663=CARTESIAN_POINT('',(-8.,-9.79717439317883E-16,-13.));
#32664=CARTESIAN_POINT('Origin',(0.,0.,-13.));
#32665=CARTESIAN_POINT('',(-8.,-9.79717439317883E-16,-12.9746));
#32666=CARTESIAN_POINT('',(-8.,-9.79717439317883E-16,-25.0375057290932));
#32667=CARTESIAN_POINT('',(8.,9.79717439317883E-16,-12.9746));
#32668=CARTESIAN_POINT('Origin',(0.,0.,-12.9746));
#32669=CARTESIAN_POINT('Origin',(0.,0.,-12.9746));
#32670=CARTESIAN_POINT('Origin',(0.,0.,-12.9746));
#32671=CARTESIAN_POINT('',(-7.,8.57252759403147E-16,-12.2743924617903));
#32672=CARTESIAN_POINT('',(7.,-8.57252759403147E-16,-12.2743924617903));
#32673=CARTESIAN_POINT('Origin',(0.,0.,-12.2743924617903));
#32674=CARTESIAN_POINT('',(8.,-9.79717439317883E-16,-12.9746));
#32675=CARTESIAN_POINT('Origin',(0.,0.,-12.2743924617903));
#32676=CARTESIAN_POINT('Origin',(0.,0.,-0.770228292030679));
#32677=CARTESIAN_POINT('',(-7.,-8.57252759403147E-16,-0.700207538209708));
#32678=CARTESIAN_POINT('Origin',(0.,0.,-0.700207538209708));
#32679=CARTESIAN_POINT('',(-8.,-9.79717439317883E-16,4.44089209850063E-15));
#32680=CARTESIAN_POINT('',(-6.9,-8.45006291411674E-16,-0.770228292030679));
#32681=CARTESIAN_POINT('Origin',(0.,0.,3.46944695195361E-15));
#32682=CARTESIAN_POINT('Origin',(0.,0.,-13.));
#32683=CARTESIAN_POINT('',(-7.,-8.57252759403147E-16,-13.));
#32684=CARTESIAN_POINT('Origin',(-3.60150143354614E-16,15.5884572681199,
-13.));
#32685=CARTESIAN_POINT('',(-13.5,7.79422863405999,-11.7942286340599));
#32686=CARTESIAN_POINT('',(-13.5,7.79422863405993,-1.20577136594005));
#32687=CARTESIAN_POINT('',(-13.5,7.79422863405993,-13.));
#32688=CARTESIAN_POINT('',(-6.75000000000002,11.6913429510899,0.));
#32689=CARTESIAN_POINT('Ctrl Pts',(-13.5000000000255,7.79422863404522,-1.20577136594854));
#32690=CARTESIAN_POINT('Ctrl Pts',(-9.8826859021901,9.88268590217392,3.5527136788005E-15));
#32691=CARTESIAN_POINT('Ctrl Pts',(-6.75000000000002,11.6913429510899,3.27551107229086E-15));
#32692=CARTESIAN_POINT('',(-8.67361737988404E-16,15.5884572681199,-1.20577136594007));
#32693=CARTESIAN_POINT('Ctrl Pts',(-6.75000000000002,11.6913429510899,3.27551107229086E-15));
#32694=CARTESIAN_POINT('Ctrl Pts',(-3.61731409780992,13.5000000000059,3.03751290454254E-15));
#32695=CARTESIAN_POINT('Ctrl Pts',(2.54925766410204E-11,15.5884572681346,
-1.20577136594856));
#32696=CARTESIAN_POINT('',(-8.67361737988404E-16,15.5884572681199,-11.7942286340599));
#32697=CARTESIAN_POINT('',(-3.60150143354614E-16,15.5884572681199,-13.));
#32698=CARTESIAN_POINT('',(-6.75000000000002,11.6913429510899,-13.));
#32699=CARTESIAN_POINT('Ctrl Pts',(-6.75000000000006,11.6913429510899,-13.));
#32700=CARTESIAN_POINT('Ctrl Pts',(-3.61731409780995,13.5000000000059,-13.));
#32701=CARTESIAN_POINT('Ctrl Pts',(2.54744281526666E-11,15.5884572681346,
-11.7942286340514));
#32702=CARTESIAN_POINT('Ctrl Pts',(-13.5000000000254,7.79422863404524,-11.7942286340515));
#32703=CARTESIAN_POINT('Ctrl Pts',(-9.8826859021901,9.88268590217391,-13.));
#32704=CARTESIAN_POINT('Ctrl Pts',(-6.75000000000006,11.6913429510899,-13.));
#32705=CARTESIAN_POINT('Origin',(13.5,7.79422863405994,-13.));
#32706=CARTESIAN_POINT('',(6.75000000000002,11.6913429510899,0.));
#32707=CARTESIAN_POINT('Ctrl Pts',(-2.5481990022814E-11,15.5884572681346,
-1.20577136594856));
#32708=CARTESIAN_POINT('Ctrl Pts',(3.61731409780993,13.5000000000059,1.22124532708767E-15));
#32709=CARTESIAN_POINT('Ctrl Pts',(6.75000000000003,11.6913429510899,-9.35860306368824E-16));
#32710=CARTESIAN_POINT('',(13.5,7.79422863405998,-1.20577136594007));
#32711=CARTESIAN_POINT('Ctrl Pts',(6.75000000000003,11.6913429510899,-9.35860306368824E-16));
#32712=CARTESIAN_POINT('Ctrl Pts',(9.8826859021901,9.88268590217392,-3.16615028890809E-15));
#32713=CARTESIAN_POINT('Ctrl Pts',(13.5000000000255,7.79422863404523,-1.20577136594854));
#32714=CARTESIAN_POINT('',(13.5,7.79422863405998,-11.7942286340599));
#32715=CARTESIAN_POINT('',(13.5,7.79422863405994,-13.));
#32716=CARTESIAN_POINT('',(6.75000000000002,11.6913429510899,-13.));
#32717=CARTESIAN_POINT('Ctrl Pts',(6.75000000000002,11.6913429510899,-13.));
#32718=CARTESIAN_POINT('Ctrl Pts',(9.88268590219009,9.88268590217393,-13.));
#32719=CARTESIAN_POINT('Ctrl Pts',(13.5000000000255,7.79422863404524,-11.7942286340515));
#32720=CARTESIAN_POINT('Ctrl Pts',(-2.54467012954593E-11,15.5884572681346,
-11.7942286340515));
#32721=CARTESIAN_POINT('Ctrl Pts',(3.61731409780994,13.5000000000059,-13.));
#32722=CARTESIAN_POINT('Ctrl Pts',(6.75000000000002,11.6913429510899,-13.));
#32723=CARTESIAN_POINT('Origin',(13.5,7.79422863405994,-13.));
#32724=CARTESIAN_POINT('',(13.5,-7.79422863405998,-1.20577136594007));
#32725=CARTESIAN_POINT('',(13.5,0.,0.));
#32726=CARTESIAN_POINT('Ctrl Pts',(13.5,-7.79422863408939,-1.20577136594856));
#32727=CARTESIAN_POINT('Ctrl Pts',(13.5,-3.61731409783199,-2.1094237467878E-15));
#32728=CARTESIAN_POINT('Ctrl Pts',(13.5,0.,-2.33965076592205E-15));
#32729=CARTESIAN_POINT('',(13.5,-7.79422863405998,-11.7942286340599));
#32730=CARTESIAN_POINT('',(13.5,-7.79422863405998,-13.));
#32731=CARTESIAN_POINT('',(13.5,0.,-13.));
#32732=CARTESIAN_POINT('Ctrl Pts',(13.5,-7.79422863408946,-11.7942286340514));
#32733=CARTESIAN_POINT('Ctrl Pts',(13.5,-3.61731409783202,-13.));
#32734=CARTESIAN_POINT('Ctrl Pts',(13.5,0.,-13.));
#32735=CARTESIAN_POINT('Ctrl Pts',(13.5,0.,-13.));
#32736=CARTESIAN_POINT('Ctrl Pts',(13.5,3.617314097832,-13.));
#32737=CARTESIAN_POINT('Ctrl Pts',(13.5,7.79422863408941,-11.7942286340514));
#32738=CARTESIAN_POINT('Ctrl Pts',(13.5,0.,-2.33965076592205E-15));
#32739=CARTESIAN_POINT('Ctrl Pts',(13.5,3.617314097832,-2.29321602408394E-15));
#32740=CARTESIAN_POINT('Ctrl Pts',(13.5,7.79422863408942,-1.20577136594857));
#32741=CARTESIAN_POINT('Origin',(2.2354950088892E-15,-15.5884572681199,
-13.));
#32742=CARTESIAN_POINT('',(6.75000000000002,-11.6913429510899,0.));
#32743=CARTESIAN_POINT('Ctrl Pts',(13.5000000000255,-7.79422863404527,-1.20577136594856));
#32744=CARTESIAN_POINT('Ctrl Pts',(9.88268590219011,-9.88268590217396,-2.1538326677728E-14));
#32745=CARTESIAN_POINT('Ctrl Pts',(6.75000000000003,-11.69134295109,-2.03549616635218E-14));
#32746=CARTESIAN_POINT('',(-5.72458747072346E-14,-15.5884572681199,-1.20577136594007));
#32747=CARTESIAN_POINT('Ctrl Pts',(6.75000000000003,-11.69134295109,-2.03549616635218E-14));
#32748=CARTESIAN_POINT('Ctrl Pts',(3.61731409780992,-13.500000000006,-1.8826547469893E-14));
#32749=CARTESIAN_POINT('Ctrl Pts',(-2.55036673839034E-11,-15.5884572681347,
-1.20577136594859));
#32750=CARTESIAN_POINT('',(-5.72458747072346E-14,-15.5884572681199,-11.7942286340599));
#32751=CARTESIAN_POINT('',(2.2354950088892E-15,-15.5884572681199,-13.));
#32752=CARTESIAN_POINT('',(6.75000000000002,-11.6913429510899,-13.));
#32753=CARTESIAN_POINT('Ctrl Pts',(6.75000000000008,-11.6913429510899,-13.));
#32754=CARTESIAN_POINT('Ctrl Pts',(3.61731409780995,-13.5000000000059,-13.));
#32755=CARTESIAN_POINT('Ctrl Pts',(-2.55021550098739E-11,-15.5884572681347,
-11.7942286340514));
#32756=CARTESIAN_POINT('Ctrl Pts',(13.5000000000255,-7.79422863404526,-11.7942286340514));
#32757=CARTESIAN_POINT('Ctrl Pts',(9.88268590219014,-9.88268590217394,-13.));
#32758=CARTESIAN_POINT('Ctrl Pts',(6.75000000000008,-11.6913429510899,-13.));
#32759=CARTESIAN_POINT('Origin',(-13.5,-7.79422863405998,-13.));
#32760=CARTESIAN_POINT('',(-6.75000000000002,-11.6913429510899,0.));
#32761=CARTESIAN_POINT('Ctrl Pts',(2.54255280590466E-11,-15.5884572681346,
-1.20577136594856));
#32762=CARTESIAN_POINT('Ctrl Pts',(-3.61731409780995,-13.5000000000059,
-1.96509475358653E-14));
#32763=CARTESIAN_POINT('Ctrl Pts',(-6.75000000000003,-11.6913429510899,
-1.98870315103374E-14));
#32764=CARTESIAN_POINT('',(-13.5,-7.79422863405999,-1.20577136594007));
#32765=CARTESIAN_POINT('Ctrl Pts',(-6.75000000000003,-11.6913429510899,
-1.98870315103374E-14));
#32766=CARTESIAN_POINT('Ctrl Pts',(-9.8826859021901,-9.88268590217396,-1.9578830969301E-14));
#32767=CARTESIAN_POINT('Ctrl Pts',(-13.5000000000255,-7.79422863404527,
-1.20577136594856));
#32768=CARTESIAN_POINT('',(-13.5,-7.79422863405999,-11.7942286340599));
#32769=CARTESIAN_POINT('',(-13.5,-7.79422863405998,-13.));
#32770=CARTESIAN_POINT('',(-6.75000000000002,-11.6913429510899,-13.));
#32771=CARTESIAN_POINT('Ctrl Pts',(-6.75000000000005,-11.6913429510899,
-13.));
#32772=CARTESIAN_POINT('Ctrl Pts',(-9.88268590219012,-9.88268590217395,
-13.));
#32773=CARTESIAN_POINT('Ctrl Pts',(-13.5000000000255,-7.79422863404526,
-11.7942286340514));
#32774=CARTESIAN_POINT('Ctrl Pts',(2.54068754460162E-11,-15.5884572681346,
-11.7942286340514));
#32775=CARTESIAN_POINT('Ctrl Pts',(-3.61731409780997,-13.5000000000059,
-13.));
#32776=CARTESIAN_POINT('Ctrl Pts',(-6.75000000000005,-11.6913429510899,
-13.));
#32777=CARTESIAN_POINT('Origin',(-13.5,7.79422863405993,-13.));
#32778=CARTESIAN_POINT('',(-13.5,0.,0.));
#32779=CARTESIAN_POINT('Ctrl Pts',(-13.5,-7.7942286340894,-1.20577136594856));
#32780=CARTESIAN_POINT('Ctrl Pts',(-13.5,-3.61731409783199,3.66373598126302E-15));
#32781=CARTESIAN_POINT('Ctrl Pts',(-13.5,7.48688245095054E-15,2.33965076592204E-15));
#32782=CARTESIAN_POINT('Ctrl Pts',(-13.5,7.48688245095054E-15,2.33965076592204E-15));
#32783=CARTESIAN_POINT('Ctrl Pts',(-13.5,3.61731409783197,9.09299790684234E-16));
#32784=CARTESIAN_POINT('Ctrl Pts',(-13.5,7.79422863408933,-1.20577136594854));
#32785=CARTESIAN_POINT('',(-13.5,0.,-13.));
#32786=CARTESIAN_POINT('Ctrl Pts',(-13.5,1.68454855146387E-14,-13.));
#32787=CARTESIAN_POINT('Ctrl Pts',(-13.5,3.61731409783201,-13.));
#32788=CARTESIAN_POINT('Ctrl Pts',(-13.5,7.79422863408941,-11.7942286340514));
#32789=CARTESIAN_POINT('Ctrl Pts',(-13.5,-7.7942286340894,-11.7942286340514));
#32790=CARTESIAN_POINT('Ctrl Pts',(-13.5,-3.61731409783199,-13.));
#32791=CARTESIAN_POINT('Ctrl Pts',(-13.5,1.68454855146387E-14,-13.));
#32792=CARTESIAN_POINT('Origin',(-1.73472347597681E-15,15.5884572681199,
0.));
#32793=CARTESIAN_POINT('Origin',(0.,0.,0.));
#32794=CARTESIAN_POINT('Origin',(0.,0.,0.));
#32795=CARTESIAN_POINT('Origin',(0.,0.,0.));
#32796=CARTESIAN_POINT('Origin',(0.,0.,0.));
#32797=CARTESIAN_POINT('Origin',(0.,0.,0.));
#32798=CARTESIAN_POINT('Origin',(0.,0.,0.));
#32799=CARTESIAN_POINT('Origin',(-1.73472347597681E-15,15.5884572681199,
-13.));
#32800=CARTESIAN_POINT('Origin',(0.,0.,-13.));
#32801=CARTESIAN_POINT('Origin',(0.,0.,-13.));
#32802=CARTESIAN_POINT('Origin',(0.,0.,-13.));
#32803=CARTESIAN_POINT('Origin',(0.,0.,-13.));
#32804=CARTESIAN_POINT('Origin',(0.,0.,-13.));
#32805=CARTESIAN_POINT('Origin',(0.,0.,-13.));
#32806=CARTESIAN_POINT('Origin',(0.,0.,-13.));
#32807=CARTESIAN_POINT('Origin',(0.,0.,-13.));
#32808=CARTESIAN_POINT('Origin',(0.,0.,-13.));
#32809=CARTESIAN_POINT('Origin',(0.,0.,-13.));
#32810=CARTESIAN_POINT('Origin',(0.,0.,-13.));
#32811=CARTESIAN_POINT('Origin',(0.,0.,-13.));
#32812=CARTESIAN_POINT('Origin',(0.,0.,0.));
#32813=CARTESIAN_POINT('Origin',(0.,0.,0.));
#32814=CARTESIAN_POINT('Origin',(0.,0.,0.));
#32815=CARTESIAN_POINT('Origin',(0.,0.,0.));
#32816=CARTESIAN_POINT('Origin',(0.,0.,0.));
#32817=CARTESIAN_POINT('Origin',(0.,0.,0.));
#32818=CARTESIAN_POINT('',(0.,0.,0.));
#32819=CARTESIAN_POINT('',(-8.32667268468867E-14,284.8125,-480.5));
#32820=CARTESIAN_POINT('',(2.09797395742799E-13,2.54098374803443E-14,63.2000000000014));
#32821=CARTESIAN_POINT('',(0.,-573.25,-15.875));
#32822=CARTESIAN_POINT('',(442.499999999986,294.8125,-970.00000000001));
#32823=CARTESIAN_POINT('',(-442.499999999999,261.000000000006,-970.699999999998));
#32824=CARTESIAN_POINT('',(442.5,244.999999999993,-970.700000000001));
#32825=CARTESIAN_POINT('',(442.499999999989,294.8125,-770.00000000001));
#32826=CARTESIAN_POINT('',(442.499999999992,294.8125,-570.00000000001));
#32827=CARTESIAN_POINT('',(-442.500000000011,294.8125,-770.));
#32828=CARTESIAN_POINT('',(-442.5,294.8125,-970.));
#32829=CARTESIAN_POINT('',(442.499999999995,294.8125,-370.00000000001));
#32830=CARTESIAN_POINT('',(442.499999999997,294.8125,-170.000000000009));
#32831=CARTESIAN_POINT('',(442.5,294.8125,29.9999999999905));
#32832=CARTESIAN_POINT('',(265.5,294.8125,29.9999999999926));
#32833=CARTESIAN_POINT('',(88.5000000000001,294.8125,29.9999999999943));
#32834=CARTESIAN_POINT('',(-88.4999999999998,294.8125,29.9999999999961));
#32835=CARTESIAN_POINT('',(-442.500000000003,294.8125,-170.));
#32836=CARTESIAN_POINT('',(-265.5,294.8125,29.9999999999979));
#32837=CARTESIAN_POINT('',(-442.5,294.8125,29.9999999999999));
#32838=CARTESIAN_POINT('',(-442.500000000006,294.8125,-370.));
#32839=CARTESIAN_POINT('',(-442.500000000009,294.8125,-570.));
#32840=CARTESIAN_POINT('',(-442.499999999997,261.000000000005,-770.524999999998));
#32841=CARTESIAN_POINT('',(-442.499999999995,261.000000000004,-570.349999999998));
#32842=CARTESIAN_POINT('',(-442.499999999993,261.000000000003,-370.174999999998));
#32843=CARTESIAN_POINT('',(-442.499999999999,261.000000000002,-169.999999999998));
#32844=CARTESIAN_POINT('',(-442.499999999999,261.000000000001,30.0000000000021));
#32845=CARTESIAN_POINT('',(-265.499999999999,261.,30.0000000000021));
#32846=CARTESIAN_POINT('',(-88.4999999999995,261.,30.0000000000021));
#32847=CARTESIAN_POINT('',(88.5000000000005,260.999999999999,30.0000000000021));
#32848=CARTESIAN_POINT('',(265.500000000001,260.999999999999,30.0000000000021));
#32849=CARTESIAN_POINT('',(442.500000000001,260.999999999998,30.0000000000021));
#32850=CARTESIAN_POINT('',(442.500000000001,260.999999999999,-169.999999999998));
#32851=CARTESIAN_POINT('',(442.499999999994,261.,-370.174999999998));
#32852=CARTESIAN_POINT('',(442.499999999997,261.000000000001,-570.349999999998));
#32853=CARTESIAN_POINT('',(442.499999999999,261.000000000003,-770.524999999998));
#32854=CARTESIAN_POINT('',(442.500000000001,261.000000000004,-970.699999999998));
#32855=CARTESIAN_POINT('',(442.499999999998,244.999999999994,-770.525000000001));
#32856=CARTESIAN_POINT('',(442.499999999996,244.999999999995,-570.350000000001));
#32857=CARTESIAN_POINT('',(442.499999999994,244.999999999996,-370.175000000001));
#32858=CARTESIAN_POINT('',(442.5,244.999999999997,-170.000000000001));
#32859=CARTESIAN_POINT('',(442.5,244.999999999998,29.9999999999992));
#32860=CARTESIAN_POINT('',(265.5,244.999999999998,29.9999999999992));
#32861=CARTESIAN_POINT('',(88.5000000000002,244.999999999998,29.9999999999992));
#32862=CARTESIAN_POINT('',(-88.4999999999998,244.999999999998,29.9999999999992));
#32863=CARTESIAN_POINT('',(-265.5,244.999999999998,29.9999999999992));
#32864=CARTESIAN_POINT('',(-442.5,244.999999999998,29.9999999999992));
#32865=CARTESIAN_POINT('',(-442.5,244.999999999997,-170.000000000001));
#32866=CARTESIAN_POINT('',(-442.499999999993,244.999999999996,-370.175000000001));
#32867=CARTESIAN_POINT('',(-442.499999999996,244.999999999995,-570.350000000001));
#32868=CARTESIAN_POINT('',(-442.499999999998,244.999999999994,-770.525000000001));
#32869=CARTESIAN_POINT('',(-442.5,244.999999999993,-970.700000000001));
#32870=UNCERTAINTY_MEASURE_WITH_UNIT(LENGTH_MEASURE(0.01),#32904,
'DISTANCE_ACCURACY_VALUE',
'Maximum model space distance between geometric entities at asserted c
onnectivities');
#32871=UNCERTAINTY_MEASURE_WITH_UNIT(LENGTH_MEASURE(0.01),#32904,
'DISTANCE_ACCURACY_VALUE',
'Maximum model space distance between geometric entities at asserted c
onnectivities');
#32872=UNCERTAINTY_MEASURE_WITH_UNIT(LENGTH_MEASURE(0.01),#32904,
'DISTANCE_ACCURACY_VALUE',
'Maximum model space distance between geometric entities at asserted c
onnectivities');
#32873=UNCERTAINTY_MEASURE_WITH_UNIT(LENGTH_MEASURE(0.01),#32904,
'DISTANCE_ACCURACY_VALUE',
'Maximum model space distance between geometric entities at asserted c
onnectivities');
#32874=UNCERTAINTY_MEASURE_WITH_UNIT(LENGTH_MEASURE(0.01),#32904,
'DISTANCE_ACCURACY_VALUE',
'Maximum model space distance between geometric entities at asserted c
onnectivities');
#32875=UNCERTAINTY_MEASURE_WITH_UNIT(LENGTH_MEASURE(0.01),#32904,
'DISTANCE_ACCURACY_VALUE',
'Maximum model space distance between geometric entities at asserted c
onnectivities');
#32876=UNCERTAINTY_MEASURE_WITH_UNIT(LENGTH_MEASURE(0.01),#32904,
'DISTANCE_ACCURACY_VALUE',
'Maximum model space distance between geometric entities at asserted c
onnectivities');
#32877=UNCERTAINTY_MEASURE_WITH_UNIT(LENGTH_MEASURE(0.01),#32904,
'DISTANCE_ACCURACY_VALUE',
'Maximum model space distance between geometric entities at asserted c
onnectivities');
#32878=UNCERTAINTY_MEASURE_WITH_UNIT(LENGTH_MEASURE(0.01),#32904,
'DISTANCE_ACCURACY_VALUE',
'Maximum model space distance between geometric entities at asserted c
onnectivities');
#32879=UNCERTAINTY_MEASURE_WITH_UNIT(LENGTH_MEASURE(0.01),#32904,
'DISTANCE_ACCURACY_VALUE',
'Maximum model space distance between geometric entities at asserted c
onnectivities');
#32880=UNCERTAINTY_MEASURE_WITH_UNIT(LENGTH_MEASURE(0.01),#32904,
'DISTANCE_ACCURACY_VALUE',
'Maximum model space distance between geometric entities at asserted c
onnectivities');
#32881=UNCERTAINTY_MEASURE_WITH_UNIT(LENGTH_MEASURE(0.01),#32904,
'DISTANCE_ACCURACY_VALUE',
'Maximum model space distance between geometric entities at asserted c
onnectivities');
#32882=UNCERTAINTY_MEASURE_WITH_UNIT(LENGTH_MEASURE(0.01),#32904,
'DISTANCE_ACCURACY_VALUE',
'Maximum model space distance between geometric entities at asserted c
onnectivities');
#32883=UNCERTAINTY_MEASURE_WITH_UNIT(LENGTH_MEASURE(0.01),#32904,
'DISTANCE_ACCURACY_VALUE',
'Maximum model space distance between geometric entities at asserted c
onnectivities');
#32884=UNCERTAINTY_MEASURE_WITH_UNIT(LENGTH_MEASURE(0.01),#32904,
'DISTANCE_ACCURACY_VALUE',
'Maximum model space distance between geometric entities at asserted c
onnectivities');
#32885=UNCERTAINTY_MEASURE_WITH_UNIT(LENGTH_MEASURE(0.01),#32904,
'DISTANCE_ACCURACY_VALUE',
'Maximum model space distance between geometric entities at asserted c
onnectivities');
#32886=UNCERTAINTY_MEASURE_WITH_UNIT(LENGTH_MEASURE(0.01),#32904,
'DISTANCE_ACCURACY_VALUE',
'Maximum model space distance between geometric entities at asserted c
onnectivities');
#32887=(
GEOMETRIC_REPRESENTATION_CONTEXT(3)
GLOBAL_UNCERTAINTY_ASSIGNED_CONTEXT((#32870))
GLOBAL_UNIT_ASSIGNED_CONTEXT((#32904,#32906,#32907))
REPRESENTATION_CONTEXT('','3D')
);
#32888=(
GEOMETRIC_REPRESENTATION_CONTEXT(3)
GLOBAL_UNCERTAINTY_ASSIGNED_CONTEXT((#32871))
GLOBAL_UNIT_ASSIGNED_CONTEXT((#32904,#32906,#32907))
REPRESENTATION_CONTEXT('','3D')
);
#32889=(
GEOMETRIC_REPRESENTATION_CONTEXT(3)
GLOBAL_UNCERTAINTY_ASSIGNED_CONTEXT((#32872))
GLOBAL_UNIT_ASSIGNED_CONTEXT((#32904,#32906,#32907))
REPRESENTATION_CONTEXT('','3D')
);
#32890=(
GEOMETRIC_REPRESENTATION_CONTEXT(3)
GLOBAL_UNCERTAINTY_ASSIGNED_CONTEXT((#32873))
GLOBAL_UNIT_ASSIGNED_CONTEXT((#32904,#32906,#32907))
REPRESENTATION_CONTEXT('','3D')
);
#32891=(
GEOMETRIC_REPRESENTATION_CONTEXT(3)
GLOBAL_UNCERTAINTY_ASSIGNED_CONTEXT((#32874))
GLOBAL_UNIT_ASSIGNED_CONTEXT((#32904,#32906,#32907))
REPRESENTATION_CONTEXT('','3D')
);
#32892=(
GEOMETRIC_REPRESENTATION_CONTEXT(3)
GLOBAL_UNCERTAINTY_ASSIGNED_CONTEXT((#32875))
GLOBAL_UNIT_ASSIGNED_CONTEXT((#32904,#32906,#32907))
REPRESENTATION_CONTEXT('','3D')
);
#32893=(
GEOMETRIC_REPRESENTATION_CONTEXT(3)
GLOBAL_UNCERTAINTY_ASSIGNED_CONTEXT((#32876))
GLOBAL_UNIT_ASSIGNED_CONTEXT((#32904,#32906,#32907))
REPRESENTATION_CONTEXT('','3D')
);
#32894=(
GEOMETRIC_REPRESENTATION_CONTEXT(3)
GLOBAL_UNCERTAINTY_ASSIGNED_CONTEXT((#32877))
GLOBAL_UNIT_ASSIGNED_CONTEXT((#32904,#32906,#32907))
REPRESENTATION_CONTEXT('','3D')
);
#32895=(
GEOMETRIC_REPRESENTATION_CONTEXT(3)
GLOBAL_UNCERTAINTY_ASSIGNED_CONTEXT((#32878))
GLOBAL_UNIT_ASSIGNED_CONTEXT((#32904,#32906,#32907))
REPRESENTATION_CONTEXT('','3D')
);
#32896=(
GEOMETRIC_REPRESENTATION_CONTEXT(3)
GLOBAL_UNCERTAINTY_ASSIGNED_CONTEXT((#32879))
GLOBAL_UNIT_ASSIGNED_CONTEXT((#32904,#32906,#32907))
REPRESENTATION_CONTEXT('','3D')
);
#32897=(
GEOMETRIC_REPRESENTATION_CONTEXT(3)
GLOBAL_UNCERTAINTY_ASSIGNED_CONTEXT((#32880))
GLOBAL_UNIT_ASSIGNED_CONTEXT((#32904,#32906,#32907))
REPRESENTATION_CONTEXT('','3D')
);
#32898=(
GEOMETRIC_REPRESENTATION_CONTEXT(3)
GLOBAL_UNCERTAINTY_ASSIGNED_CONTEXT((#32881))
GLOBAL_UNIT_ASSIGNED_CONTEXT((#32904,#32906,#32907))
REPRESENTATION_CONTEXT('','3D')
);
#32899=(
GEOMETRIC_REPRESENTATION_CONTEXT(3)
GLOBAL_UNCERTAINTY_ASSIGNED_CONTEXT((#32882))
GLOBAL_UNIT_ASSIGNED_CONTEXT((#32904,#32906,#32907))
REPRESENTATION_CONTEXT('','3D')
);
#32900=(
GEOMETRIC_REPRESENTATION_CONTEXT(3)
GLOBAL_UNCERTAINTY_ASSIGNED_CONTEXT((#32883))
GLOBAL_UNIT_ASSIGNED_CONTEXT((#32904,#32906,#32907))
REPRESENTATION_CONTEXT('','3D')
);
#32901=(
GEOMETRIC_REPRESENTATION_CONTEXT(3)
GLOBAL_UNCERTAINTY_ASSIGNED_CONTEXT((#32884))
GLOBAL_UNIT_ASSIGNED_CONTEXT((#32904,#32906,#32907))
REPRESENTATION_CONTEXT('','3D')
);
#32902=(
GEOMETRIC_REPRESENTATION_CONTEXT(3)
GLOBAL_UNCERTAINTY_ASSIGNED_CONTEXT((#32885))
GLOBAL_UNIT_ASSIGNED_CONTEXT((#32904,#32906,#32907))
REPRESENTATION_CONTEXT('','3D')
);
#32903=(
GEOMETRIC_REPRESENTATION_CONTEXT(3)
GLOBAL_UNCERTAINTY_ASSIGNED_CONTEXT((#32886))
GLOBAL_UNIT_ASSIGNED_CONTEXT((#32904,#32906,#32907))
REPRESENTATION_CONTEXT('','3D')
);
#32904=(
LENGTH_UNIT()
NAMED_UNIT(*)
SI_UNIT(.MILLI.,.METRE.)
);
#32905=(
LENGTH_UNIT()
NAMED_UNIT(*)
SI_UNIT($,.METRE.)
);
#32906=(
NAMED_UNIT(*)
PLANE_ANGLE_UNIT()
SI_UNIT($,.RADIAN.)
);
#32907=(
NAMED_UNIT(*)
SI_UNIT($,.STERADIAN.)
SOLID_ANGLE_UNIT()
);
#32908=SHAPE_DEFINITION_REPRESENTATION(#32924,#33012);
#32909=SHAPE_DEFINITION_REPRESENTATION(#32925,#33013);
#32910=SHAPE_DEFINITION_REPRESENTATION(#32926,#33014);
#32911=SHAPE_DEFINITION_REPRESENTATION(#32927,#33015);
#32912=SHAPE_DEFINITION_REPRESENTATION(#32928,#33016);
#32913=SHAPE_DEFINITION_REPRESENTATION(#32929,#33017);
#32914=SHAPE_DEFINITION_REPRESENTATION(#32930,#33018);
#32915=SHAPE_DEFINITION_REPRESENTATION(#32931,#33019);
#32916=SHAPE_DEFINITION_REPRESENTATION(#32932,#33020);
#32917=SHAPE_DEFINITION_REPRESENTATION(#32933,#33021);
#32918=SHAPE_DEFINITION_REPRESENTATION(#32934,#33022);
#32919=SHAPE_DEFINITION_REPRESENTATION(#32935,#33023);
#32920=SHAPE_DEFINITION_REPRESENTATION(#32956,#33024);
#32921=SHAPE_DEFINITION_REPRESENTATION(#32957,#33025);
#32922=SHAPE_DEFINITION_REPRESENTATION(#32958,#33026);
#32923=SHAPE_DEFINITION_REPRESENTATION(#32959,#33027);
#32924=PRODUCT_DEFINITION_SHAPE('',$,#33029);
#32925=PRODUCT_DEFINITION_SHAPE('',$,#33030);
#32926=PRODUCT_DEFINITION_SHAPE('',$,#33031);
#32927=PRODUCT_DEFINITION_SHAPE('',$,#33032);
#32928=PRODUCT_DEFINITION_SHAPE('',$,#33033);
#32929=PRODUCT_DEFINITION_SHAPE('',$,#33034);
#32930=PRODUCT_DEFINITION_SHAPE('',$,#33035);
#32931=PRODUCT_DEFINITION_SHAPE('',$,#33036);
#32932=PRODUCT_DEFINITION_SHAPE('',$,#33037);
#32933=PRODUCT_DEFINITION_SHAPE('',$,#33038);
#32934=PRODUCT_DEFINITION_SHAPE('',$,#33039);
#32935=PRODUCT_DEFINITION_SHAPE('',$,#33040);
#32936=PRODUCT_DEFINITION_SHAPE($,$,#227);
#32937=PRODUCT_DEFINITION_SHAPE($,$,#228);
#32938=PRODUCT_DEFINITION_SHAPE($,$,#229);
#32939=PRODUCT_DEFINITION_SHAPE($,$,#230);
#32940=PRODUCT_DEFINITION_SHAPE($,$,#231);
#32941=PRODUCT_DEFINITION_SHAPE($,$,#232);
#32942=PRODUCT_DEFINITION_SHAPE($,$,#233);
#32943=PRODUCT_DEFINITION_SHAPE($,$,#234);
#32944=PRODUCT_DEFINITION_SHAPE($,$,#235);
#32945=PRODUCT_DEFINITION_SHAPE($,$,#236);
#32946=PRODUCT_DEFINITION_SHAPE($,$,#237);
#32947=PRODUCT_DEFINITION_SHAPE($,$,#238);
#32948=PRODUCT_DEFINITION_SHAPE($,$,#239);
#32949=PRODUCT_DEFINITION_SHAPE($,$,#240);
#32950=PRODUCT_DEFINITION_SHAPE($,$,#241);
#32951=PRODUCT_DEFINITION_SHAPE($,$,#242);
#32952=PRODUCT_DEFINITION_SHAPE($,$,#243);
#32953=PRODUCT_DEFINITION_SHAPE($,$,#244);
#32954=PRODUCT_DEFINITION_SHAPE($,$,#245);
#32955=PRODUCT_DEFINITION_SHAPE($,$,#246);
#32956=PRODUCT_DEFINITION_SHAPE('',$,#33041);
#32957=PRODUCT_DEFINITION_SHAPE('',$,#33042);
#32958=PRODUCT_DEFINITION_SHAPE('',$,#33043);
#32959=PRODUCT_DEFINITION_SHAPE('',$,#33044);
#32960=PRODUCT_DEFINITION_SHAPE($,$,#247);
#32961=PRODUCT_DEFINITION_SHAPE($,$,#248);
#32962=PRODUCT_DEFINITION_SHAPE($,$,#249);
#32963=PRODUCT_DEFINITION_SHAPE($,$,#250);
#32964=PRODUCT_DEFINITION_SHAPE($,$,#251);
#32965=PRODUCT_DEFINITION_SHAPE($,$,#252);
#32966=PRODUCT_DEFINITION_SHAPE($,$,#253);
#32967=PRODUCT_DEFINITION_SHAPE($,$,#254);
#32968=PRODUCT_DEFINITION_SHAPE($,$,#255);
#32969=PRODUCT_DEFINITION_SHAPE($,$,#256);
#32970=PRODUCT_DEFINITION_SHAPE($,$,#257);
#32971=PRODUCT_DEFINITION_SHAPE($,$,#258);
#32972=PRODUCT_DEFINITION_SHAPE($,$,#259);
#32973=PRODUCT_DEFINITION_SHAPE($,$,#260);
#32974=PRODUCT_DEFINITION_SHAPE($,$,#261);
#32975=PRODUCT_DEFINITION_SHAPE($,$,#262);
#32976=PRODUCT_DEFINITION_SHAPE($,$,#263);
#32977=PRODUCT_DEFINITION_SHAPE($,$,#264);
#32978=PRODUCT_DEFINITION_SHAPE($,$,#265);
#32979=PRODUCT_DEFINITION_SHAPE($,$,#266);
#32980=PRODUCT_DEFINITION_SHAPE($,$,#267);
#32981=PRODUCT_DEFINITION_SHAPE($,$,#268);
#32982=PRODUCT_DEFINITION_SHAPE($,$,#269);
#32983=PRODUCT_DEFINITION_SHAPE($,$,#270);
#32984=PRODUCT_DEFINITION_SHAPE($,$,#271);
#32985=PRODUCT_DEFINITION_SHAPE($,$,#272);
#32986=PRODUCT_DEFINITION_SHAPE($,$,#273);
#32987=PRODUCT_DEFINITION_SHAPE($,$,#274);
#32988=PRODUCT_DEFINITION_SHAPE($,$,#275);
#32989=PRODUCT_DEFINITION_SHAPE($,$,#276);
#32990=PRODUCT_DEFINITION_SHAPE($,$,#277);
#32991=PRODUCT_DEFINITION_SHAPE($,$,#278);
#32992=PRODUCT_DEFINITION_SHAPE($,$,#279);
#32993=PRODUCT_DEFINITION_SHAPE($,$,#280);
#32994=PRODUCT_DEFINITION_SHAPE($,$,#281);
#32995=PRODUCT_DEFINITION_SHAPE($,$,#282);
#32996=PRODUCT_DEFINITION_SHAPE($,$,#283);
#32997=PRODUCT_DEFINITION_SHAPE($,$,#284);
#32998=PRODUCT_DEFINITION_SHAPE($,$,#285);
#32999=PRODUCT_DEFINITION_SHAPE($,$,#286);
#33000=PRODUCT_DEFINITION_SHAPE($,$,#287);
#33001=PRODUCT_DEFINITION_SHAPE($,$,#288);
#33002=PRODUCT_DEFINITION_SHAPE($,$,#289);
#33003=PRODUCT_DEFINITION_SHAPE($,$,#290);
#33004=PRODUCT_DEFINITION_SHAPE($,$,#291);
#33005=PRODUCT_DEFINITION_SHAPE($,$,#292);
#33006=PRODUCT_DEFINITION_SHAPE($,$,#293);
#33007=PRODUCT_DEFINITION_SHAPE($,$,#294);
#33008=PRODUCT_DEFINITION_SHAPE($,$,#295);
#33009=PRODUCT_DEFINITION_SHAPE($,$,#296);
#33010=PRODUCT_DEFINITION_SHAPE($,$,#297);
#33011=PRODUCT_DEFINITION_SHAPE($,$,#298);
#33012=SHAPE_REPRESENTATION('',(#15783,#17105,#17106,#17107,#17108,#17109,
#17110,#17111,#17112,#17113,#17114,#17115,#17116,#17117,#17118,#17119,#17120,
#17121,#17122,#17123,#17124,#17125,#17126,#17127,#17128,#17129,#17130,#17131,
#17132,#17133,#17134,#17135,#17136,#17137,#17138,#17139,#17140,#17141,#17142,
#17143,#17144,#17145,#17146,#17147,#17148,#17149,#17150,#17151,#17152,#17153,
#17154,#17155,#17156),#32887);
#33013=SHAPE_REPRESENTATION('',(#15784),#32888);
#33014=SHAPE_REPRESENTATION('',(#15899),#32889);
#33015=SHAPE_REPRESENTATION('',(#16040,#16528,#16529,#16530,#16531,#16532,
#16533,#16534,#16535,#16536,#16537,#16538,#16539,#16540,#16541,#16542,#16543,
#16544,#16545,#16546,#16547),#32890);
#33016=SHAPE_REPRESENTATION('',(#16041),#32891);
#33017=SHAPE_REPRESENTATION('',(#16210),#32892);
#33018=SHAPE_REPRESENTATION('',(#16276),#32893);
#33019=SHAPE_REPRESENTATION('',(#16303),#32894);
#33020=SHAPE_REPRESENTATION('',(#16330),#32895);
#33021=SHAPE_REPRESENTATION('',(#16374),#32896);
#33022=SHAPE_REPRESENTATION('',(#16451),#32897);
#33023=SHAPE_REPRESENTATION('',(#16519),#32898);
#33024=SHAPE_REPRESENTATION('',(#16548),#32899);
#33025=SHAPE_REPRESENTATION('',(#17007),#32900);
#33026=SHAPE_REPRESENTATION('',(#17052),#32901);
#33027=SHAPE_REPRESENTATION('',(#17061),#32902);
#33028=PRODUCT_DEFINITION_CONTEXT('part definition',#33078,'design');
#33029=PRODUCT_DEFINITION('MAT-033','MAT-033',#33045,#33028);
#33030=PRODUCT_DEFINITION('Head Compartment','Head Compartment',#33046,
#33028);
#33031=PRODUCT_DEFINITION('Head Cap','Head Cap',#33047,#33028);
#33032=PRODUCT_DEFINITION('Access Cover Assembly',
'Access Cover Assembly',#33048,#33028);
#33033=PRODUCT_DEFINITION('Access Door Frame','Access Door Frame',#33049,
#33028);
#33034=PRODUCT_DEFINITION('Access Door Cover','Access Door Cover',#33050,
#33028);
#33035=PRODUCT_DEFINITION('Heavy Hex Bolt 0.625-18 x 1.75 x 1.25',
'Heavy Hex Bolt 0.625-18 x 1.75 x 1.25',#33051,#33028);
#33036=PRODUCT_DEFINITION('Heavy Hex Bolt 0.625-18 x 2.5 x 1.25',
'Heavy Hex Bolt 0.625-18 x 2.5 x 1.25',#33052,#33028);
#33037=PRODUCT_DEFINITION('Hex Nut 0.625-18','Hex Nut 0.625-18',#33053,
#33028);
#33038=PRODUCT_DEFINITION('Eye Bolt','Eye Bolt',#33054,#33028);
#33039=PRODUCT_DEFINITION('Cover Clamp','Cover Clamp',#33055,#33028);
#33040=PRODUCT_DEFINITION('Narrow Flat Washer 0.625',
'Narrow Flat Washer 0.625',#33056,#33028);
#33041=PRODUCT_DEFINITION('Chute Body','Chute Body',#33057,#33028);
#33042=PRODUCT_DEFINITION(
'High Strength Hex Head Bolt DIN 6914 M16 x 60',
'High Strength Hex Head Bolt DIN 6914 M16 x 60',#33058,#33028);
#33043=PRODUCT_DEFINITION('Plain Washer DIN 125 A 17',
'Plain Washer DIN 125 A 17',#33059,#33028);
#33044=PRODUCT_DEFINITION('High Strength Hex Nut DIN 6915 M16',
'High Strength Hex Nut DIN 6915 M16',#33060,#33028);
#33045=PRODUCT_DEFINITION_FORMATION('',$,#33080);
#33046=PRODUCT_DEFINITION_FORMATION('',$,#33081);
#33047=PRODUCT_DEFINITION_FORMATION('',$,#33082);
#33048=PRODUCT_DEFINITION_FORMATION('',$,#33083);
#33049=PRODUCT_DEFINITION_FORMATION('',$,#33084);
#33050=PRODUCT_DEFINITION_FORMATION('',$,#33085);
#33051=PRODUCT_DEFINITION_FORMATION('',$,#33086);
#33052=PRODUCT_DEFINITION_FORMATION('',$,#33087);
#33053=PRODUCT_DEFINITION_FORMATION('',$,#33088);
#33054=PRODUCT_DEFINITION_FORMATION('',$,#33089);
#33055=PRODUCT_DEFINITION_FORMATION('',$,#33090);
#33056=PRODUCT_DEFINITION_FORMATION('',$,#33091);
#33057=PRODUCT_DEFINITION_FORMATION('',$,#33092);
#33058=PRODUCT_DEFINITION_FORMATION('',$,#33093);
#33059=PRODUCT_DEFINITION_FORMATION('',$,#33094);
#33060=PRODUCT_DEFINITION_FORMATION('',$,#33095);
#33061=PRODUCT_RELATED_PRODUCT_CATEGORY('MAT-033','MAT-033',(#33080));
#33062=PRODUCT_RELATED_PRODUCT_CATEGORY('Head Compartment',
'Head Compartment',(#33081));
#33063=PRODUCT_RELATED_PRODUCT_CATEGORY('Head Cap','Head Cap',(#33082));
#33064=PRODUCT_RELATED_PRODUCT_CATEGORY('Access Cover Assembly',
'Access Cover Assembly',(#33083));
#33065=PRODUCT_RELATED_PRODUCT_CATEGORY('Access Door Frame',
'Access Door Frame',(#33084));
#33066=PRODUCT_RELATED_PRODUCT_CATEGORY('Access Door Cover',
'Access Door Cover',(#33085));
#33067=PRODUCT_RELATED_PRODUCT_CATEGORY(
'Heavy Hex Bolt 0.625-18 x 1.75 x 1.25',
'Heavy Hex Bolt 0.625-18 x 1.75 x 1.25',(#33086));
#33068=PRODUCT_RELATED_PRODUCT_CATEGORY(
'Heavy Hex Bolt 0.625-18 x 2.5 x 1.25',
'Heavy Hex Bolt 0.625-18 x 2.5 x 1.25',(#33087));
#33069=PRODUCT_RELATED_PRODUCT_CATEGORY('Hex Nut 0.625-18',
'Hex Nut 0.625-18',(#33088));
#33070=PRODUCT_RELATED_PRODUCT_CATEGORY('Eye Bolt','Eye Bolt',(#33089));
#33071=PRODUCT_RELATED_PRODUCT_CATEGORY('Cover Clamp','Cover Clamp',(#33090));
#33072=PRODUCT_RELATED_PRODUCT_CATEGORY('Narrow Flat Washer 0.625',
'Narrow Flat Washer 0.625',(#33091));
#33073=PRODUCT_RELATED_PRODUCT_CATEGORY('Chute Body','Chute Body',(#33092));
#33074=PRODUCT_RELATED_PRODUCT_CATEGORY(
'High Strength Hex Head Bolt DIN 6914 M16 x 60',
'High Strength Hex Head Bolt DIN 6914 M16 x 60',(#33093));
#33075=PRODUCT_RELATED_PRODUCT_CATEGORY('Plain Washer DIN 125 A 17',
'Plain Washer DIN 125 A 17',(#33094));
#33076=PRODUCT_RELATED_PRODUCT_CATEGORY(
'High Strength Hex Nut DIN 6915 M16',
'High Strength Hex Nut DIN 6915 M16',(#33095));
#33077=APPLICATION_PROTOCOL_DEFINITION('international standard',
'automotive_design',2009,#33078);
#33078=APPLICATION_CONTEXT(
'Core Data for Automotive Mechanical Design Process');
#33079=PRODUCT_CONTEXT('part definition',#33078,'mechanical');
#33080=PRODUCT('MAT-033','MAT-033','STEP AP214',(#33079));
#33081=PRODUCT('Head Compartment','Head Compartment',$,(#33079));
#33082=PRODUCT('Head Cap','Head Cap',$,(#33079));
#33083=PRODUCT('Access Cover Assembly','Access Cover Assembly',$,(#33079));
#33084=PRODUCT('Access Door Frame','Access Door Frame',$,(#33079));
#33085=PRODUCT('Access Door Cover','Access Door Cover',$,(#33079));
#33086=PRODUCT('Heavy Hex Bolt 0.625-18 x 1.75 x 1.25',
'Heavy Hex Bolt 0.625-18 x 1.75 x 1.25',$,(#33079));
#33087=PRODUCT('Heavy Hex Bolt 0.625-18 x 2.5 x 1.25',
'Heavy Hex Bolt 0.625-18 x 2.5 x 1.25',$,(#33079));
#33088=PRODUCT('Hex Nut 0.625-18','Hex Nut 0.625-18',$,(#33079));
#33089=PRODUCT('Eye Bolt','Eye Bolt',$,(#33079));
#33090=PRODUCT('Cover Clamp','Cover Clamp',$,(#33079));
#33091=PRODUCT('Narrow Flat Washer 0.625','Narrow Flat Washer 0.625',$,
(#33079));
#33092=PRODUCT('Chute Body','Chute Body',$,(#33079));
#33093=PRODUCT('High Strength Hex Head Bolt DIN 6914 M16 x 60',
'High Strength Hex Head Bolt DIN 6914 M16 x 60',$,(#33079));
#33094=PRODUCT('Plain Washer DIN 125 A 17','Plain Washer DIN 125 A 17',
$,(#33079));
#33095=PRODUCT('High Strength Hex Nut DIN 6915 M16',
'High Strength Hex Nut DIN 6915 M16',$,(#33079));
#33096=PRESENTATION_STYLE_ASSIGNMENT((#33102));
#33097=PRESENTATION_STYLE_ASSIGNMENT((#33103));
#33098=PRESENTATION_STYLE_ASSIGNMENT((#33104));
#33099=PRESENTATION_STYLE_ASSIGNMENT((#33105));
#33100=PRESENTATION_STYLE_ASSIGNMENT((#33106));
#33101=PRESENTATION_STYLE_ASSIGNMENT((#33107));
#33102=SURFACE_STYLE_USAGE(.BOTH.,#33108);
#33103=SURFACE_STYLE_USAGE(.BOTH.,#33109);
#33104=SURFACE_STYLE_USAGE(.BOTH.,#33110);
#33105=SURFACE_STYLE_USAGE(.BOTH.,#33111);
#33106=SURFACE_STYLE_USAGE(.BOTH.,#33112);
#33107=SURFACE_STYLE_USAGE(.BOTH.,#33113);
#33108=SURFACE_SIDE_STYLE('',(#33114));
#33109=SURFACE_SIDE_STYLE('',(#33115));
#33110=SURFACE_SIDE_STYLE('',(#33116));
#33111=SURFACE_SIDE_STYLE('',(#33117));
#33112=SURFACE_SIDE_STYLE('',(#33118));
#33113=SURFACE_SIDE_STYLE('',(#33119));
#33114=SURFACE_STYLE_FILL_AREA(#33120);
#33115=SURFACE_STYLE_FILL_AREA(#33121);
#33116=SURFACE_STYLE_FILL_AREA(#33122);
#33117=SURFACE_STYLE_FILL_AREA(#33123);
#33118=SURFACE_STYLE_FILL_AREA(#33124);
#33119=SURFACE_STYLE_FILL_AREA(#33125);
#33120=FILL_AREA_STYLE('Steel - Satin',(#33126));
#33121=FILL_AREA_STYLE('Opaque(61,176,222)',(#33127));
#33122=FILL_AREA_STYLE('Opaque(227,224,212)',(#33128));
#33123=FILL_AREA_STYLE('Opaque(31,36,43)',(#33129));
#33124=FILL_AREA_STYLE('Opaque(97,158,199)',(#33130));
#33125=FILL_AREA_STYLE('Opaque(20,51,87)',(#33131));
#33126=FILL_AREA_STYLE_COLOUR('Steel - Satin',#33132);
#33127=FILL_AREA_STYLE_COLOUR('Opaque(61,176,222)',#33133);
#33128=FILL_AREA_STYLE_COLOUR('Opaque(227,224,212)',#33134);
#33129=FILL_AREA_STYLE_COLOUR('Opaque(31,36,43)',#33135);
#33130=FILL_AREA_STYLE_COLOUR('Opaque(97,158,199)',#33136);
#33131=FILL_AREA_STYLE_COLOUR('Opaque(20,51,87)',#33137);
#33132=COLOUR_RGB('Steel - Satin',0.627450980392157,0.627450980392157,0.627450980392157);
#33133=COLOUR_RGB('Opaque(61,176,222)',0.23921568627451,0.690196078431373,
0.870588235294118);
#33134=COLOUR_RGB('Opaque(227,224,212)',0.890196078431372,0.87843137254902,
0.831372549019608);
#33135=COLOUR_RGB('Opaque(31,36,43)',0.12156862745098,0.141176470588235,
0.168627450980392);
#33136=COLOUR_RGB('Opaque(97,158,199)',0.380392156862745,0.619607843137255,
0.780392156862745);
#33137=COLOUR_RGB('Opaque(20,51,87)',0.0784313725490196,0.2,0.341176470588235);
ENDSEC;
END-ISO-10303-21;
